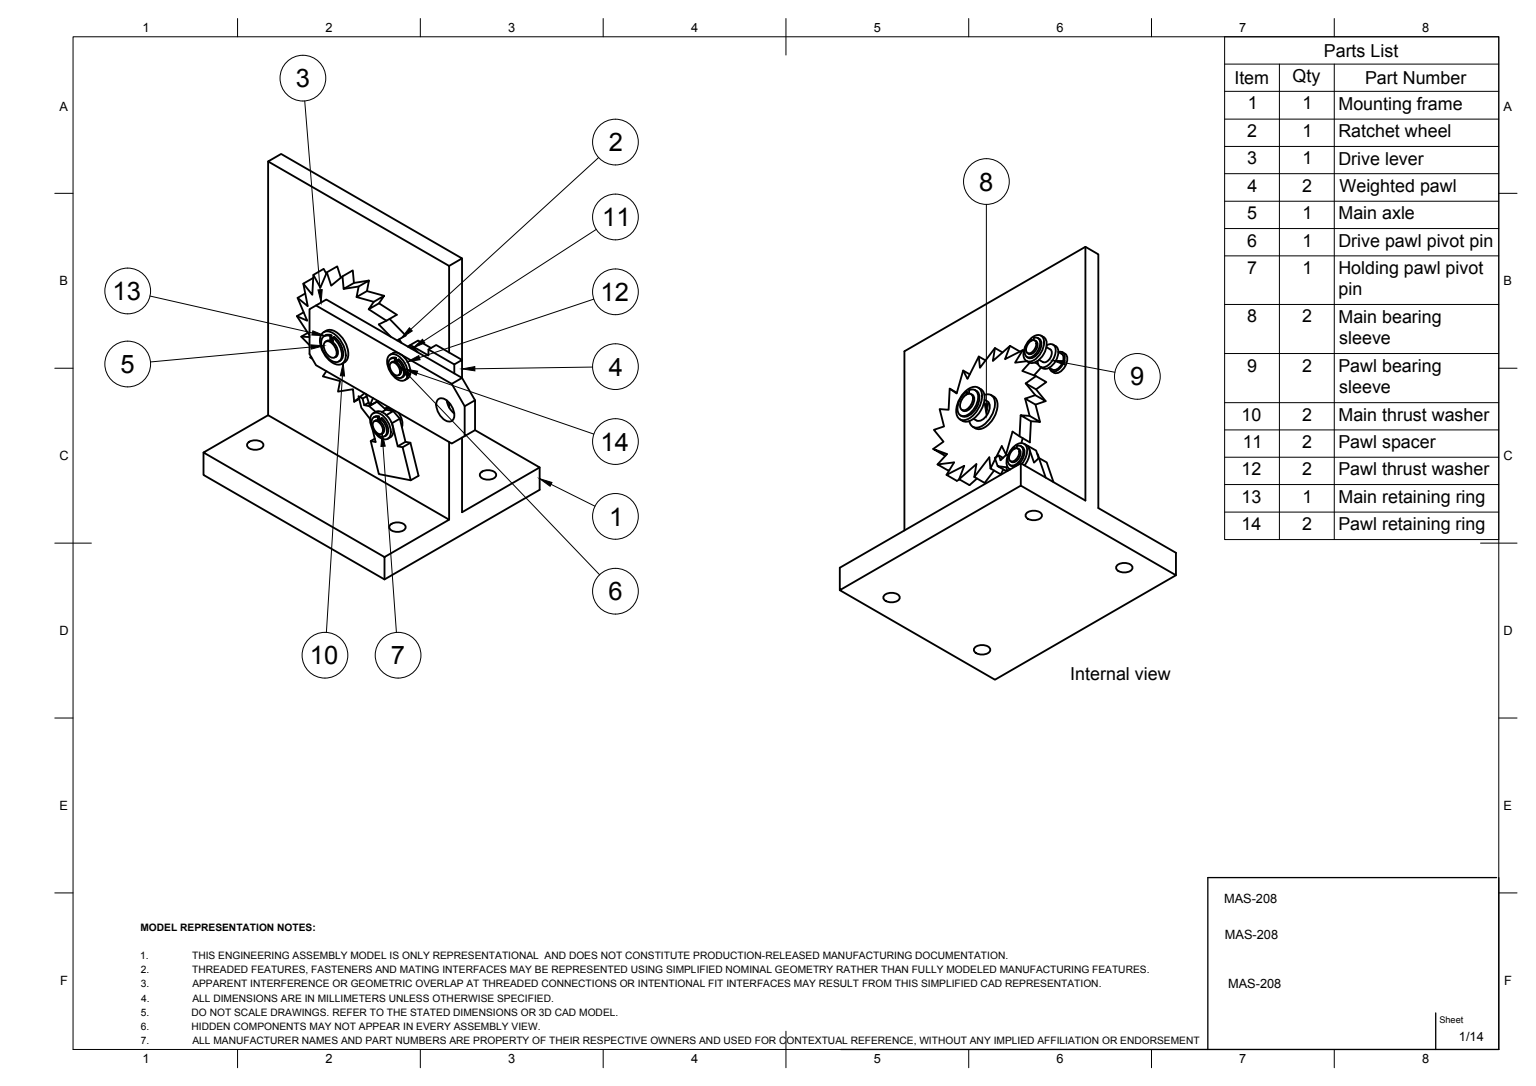
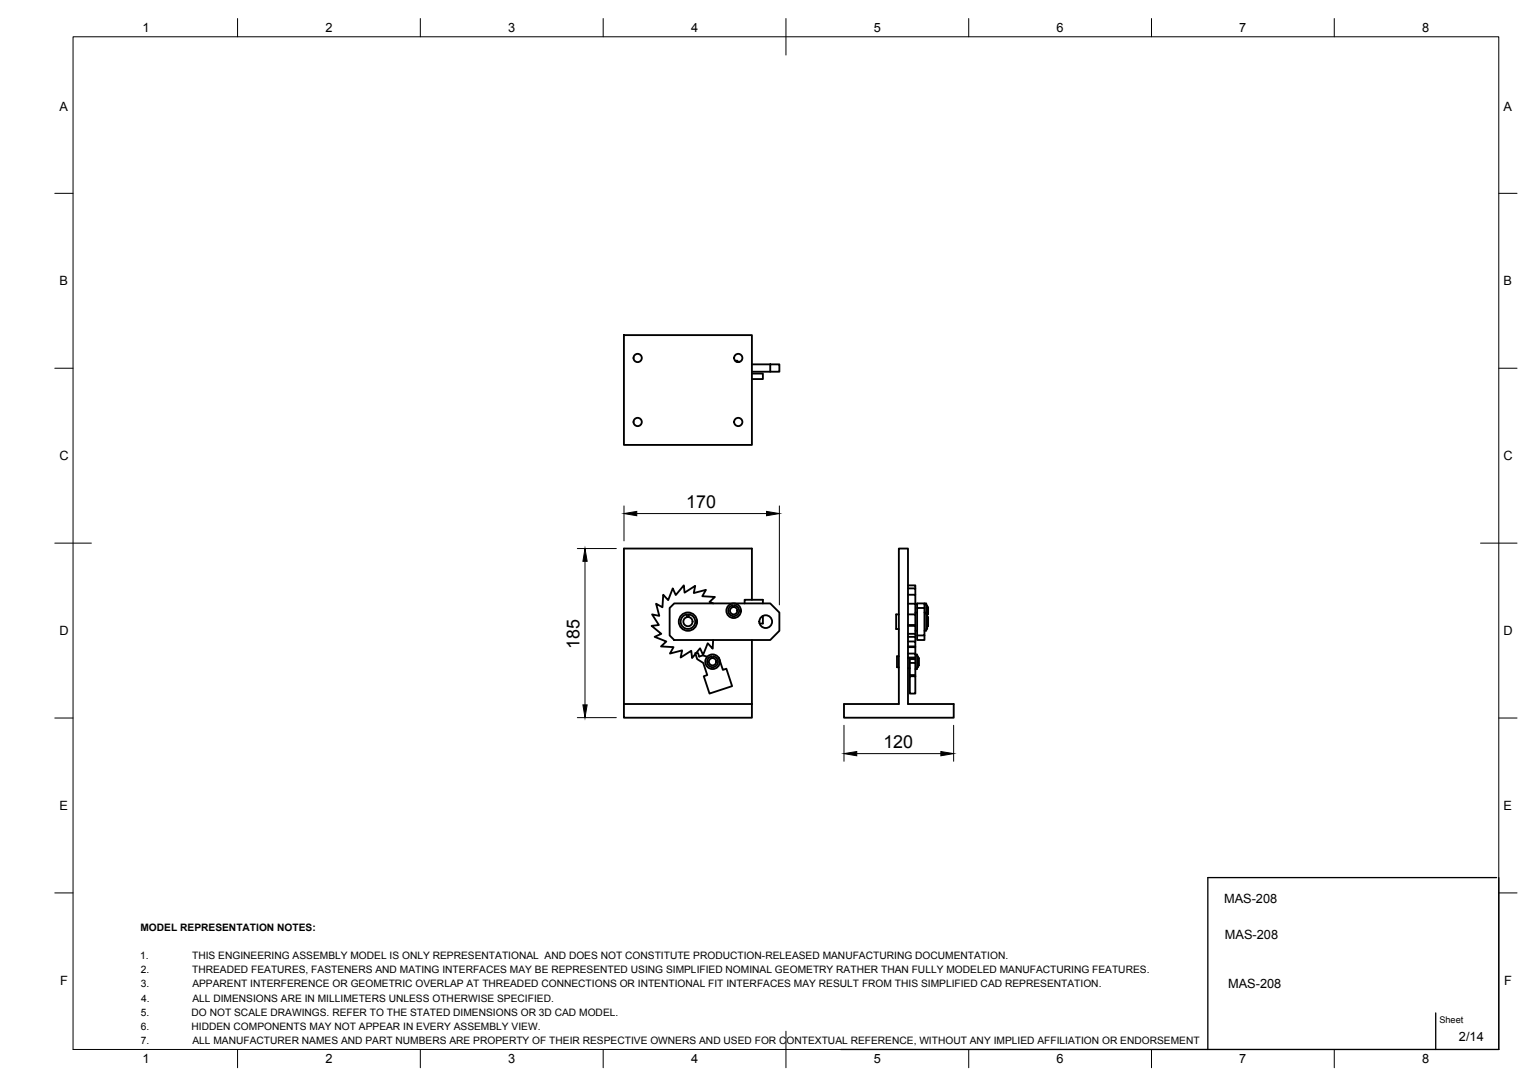
ISO-10303-21;
HEADER;
/* Generated by software containing ST-Developer
 * from STEP Tools, Inc. (www.steptools.com) 
 */

FILE_DESCRIPTION(
/* description */ ('Independent vertical20-tooth ratchet advance with repeated integral-c
ounterweight gravity pawls, swinging drive lever, bronze sleeves and f
ully retained axle stacks.18degpertooth. Native revolutes; geometric c
ycle checking rather than automatic contact/rolling dynamics. Gravity 
closing checked from actual pawl center of mass. Backplate/foot suppor
ts unit. Fits, torque, holding force, wear and life unassigned.'),
/* implementation_level */ '2;1');

FILE_NAME(
/* name */ 'MAS-208.step',
/* time_stamp */ '2026-11-09T06:25:53-08:00',
/* author */ (''),
/* organization */ (''),
/* preprocessor_version */ 'ST-DEVELOPER v20.2',
/* originating_system */ 'Autodesk Translation Framework v15.17.0.0',
/* authorisation */ '');

FILE_SCHEMA (('AUTOMOTIVE_DESIGN { 1 0 10303 214 3 1 1 }'));
ENDSEC;

DATA;
#10=MECHANICAL_DESIGN_GEOMETRIC_PRESENTATION_REPRESENTATION('',(#123,#124,
#125,#126,#127,#128,#129,#130,#131,#132,#133,#134,#135,#136),#4643);
#11=ITEM_DEFINED_TRANSFORMATION($,$,#2829,#3066);
#12=ITEM_DEFINED_TRANSFORMATION($,$,#2858,#3067);
#13=ITEM_DEFINED_TRANSFORMATION($,$,#2904,#3068);
#14=ITEM_DEFINED_TRANSFORMATION($,$,#2989,#3069);
#15=ITEM_DEFINED_TRANSFORMATION($,$,#2924,#3070);
#16=ITEM_DEFINED_TRANSFORMATION($,$,#2942,#3071);
#17=ITEM_DEFINED_TRANSFORMATION($,$,#2960,#3072);
#18=ITEM_DEFINED_TRANSFORMATION($,$,#3010,#3073);
#19=ITEM_DEFINED_TRANSFORMATION($,$,#3019,#3074);
#20=ITEM_DEFINED_TRANSFORMATION($,$,#3028,#3075);
#21=ITEM_DEFINED_TRANSFORMATION($,$,#3037,#3076);
#22=ITEM_DEFINED_TRANSFORMATION($,$,#3046,#3077);
#23=ITEM_DEFINED_TRANSFORMATION($,$,#2978,#3078);
#24=ITEM_DEFINED_TRANSFORMATION($,$,#3055,#3079);
#25=ITEM_DEFINED_TRANSFORMATION($,$,#2989,#3080);
#26=ITEM_DEFINED_TRANSFORMATION($,$,#3010,#3081);
#27=ITEM_DEFINED_TRANSFORMATION($,$,#3019,#3082);
#28=ITEM_DEFINED_TRANSFORMATION($,$,#3028,#3083);
#29=ITEM_DEFINED_TRANSFORMATION($,$,#3037,#3084);
#30=ITEM_DEFINED_TRANSFORMATION($,$,#3046,#3085);
#31=ITEM_DEFINED_TRANSFORMATION($,$,#3055,#3086);
#32=(
REPRESENTATION_RELATIONSHIP($,$,#4700,#4699)
REPRESENTATION_RELATIONSHIP_WITH_TRANSFORMATION(#11)
SHAPE_REPRESENTATION_RELATIONSHIP()
);
#33=(
REPRESENTATION_RELATIONSHIP($,$,#4701,#4699)
REPRESENTATION_RELATIONSHIP_WITH_TRANSFORMATION(#12)
SHAPE_REPRESENTATION_RELATIONSHIP()
);
#34=(
REPRESENTATION_RELATIONSHIP($,$,#4702,#4699)
REPRESENTATION_RELATIONSHIP_WITH_TRANSFORMATION(#13)
SHAPE_REPRESENTATION_RELATIONSHIP()
);
#35=(
REPRESENTATION_RELATIONSHIP($,$,#4707,#4699)
REPRESENTATION_RELATIONSHIP_WITH_TRANSFORMATION(#14)
SHAPE_REPRESENTATION_RELATIONSHIP()
);
#36=(
REPRESENTATION_RELATIONSHIP($,$,#4703,#4699)
REPRESENTATION_RELATIONSHIP_WITH_TRANSFORMATION(#15)
SHAPE_REPRESENTATION_RELATIONSHIP()
);
#37=(
REPRESENTATION_RELATIONSHIP($,$,#4704,#4699)
REPRESENTATION_RELATIONSHIP_WITH_TRANSFORMATION(#16)
SHAPE_REPRESENTATION_RELATIONSHIP()
);
#38=(
REPRESENTATION_RELATIONSHIP($,$,#4705,#4699)
REPRESENTATION_RELATIONSHIP_WITH_TRANSFORMATION(#17)
SHAPE_REPRESENTATION_RELATIONSHIP()
);
#39=(
REPRESENTATION_RELATIONSHIP($,$,#4708,#4699)
REPRESENTATION_RELATIONSHIP_WITH_TRANSFORMATION(#18)
SHAPE_REPRESENTATION_RELATIONSHIP()
);
#40=(
REPRESENTATION_RELATIONSHIP($,$,#4709,#4699)
REPRESENTATION_RELATIONSHIP_WITH_TRANSFORMATION(#19)
SHAPE_REPRESENTATION_RELATIONSHIP()
);
#41=(
REPRESENTATION_RELATIONSHIP($,$,#4710,#4699)
REPRESENTATION_RELATIONSHIP_WITH_TRANSFORMATION(#20)
SHAPE_REPRESENTATION_RELATIONSHIP()
);
#42=(
REPRESENTATION_RELATIONSHIP($,$,#4711,#4699)
REPRESENTATION_RELATIONSHIP_WITH_TRANSFORMATION(#21)
SHAPE_REPRESENTATION_RELATIONSHIP()
);
#43=(
REPRESENTATION_RELATIONSHIP($,$,#4712,#4699)
REPRESENTATION_RELATIONSHIP_WITH_TRANSFORMATION(#22)
SHAPE_REPRESENTATION_RELATIONSHIP()
);
#44=(
REPRESENTATION_RELATIONSHIP($,$,#4706,#4699)
REPRESENTATION_RELATIONSHIP_WITH_TRANSFORMATION(#23)
SHAPE_REPRESENTATION_RELATIONSHIP()
);
#45=(
REPRESENTATION_RELATIONSHIP($,$,#4713,#4699)
REPRESENTATION_RELATIONSHIP_WITH_TRANSFORMATION(#24)
SHAPE_REPRESENTATION_RELATIONSHIP()
);
#46=(
REPRESENTATION_RELATIONSHIP($,$,#4707,#4699)
REPRESENTATION_RELATIONSHIP_WITH_TRANSFORMATION(#25)
SHAPE_REPRESENTATION_RELATIONSHIP()
);
#47=(
REPRESENTATION_RELATIONSHIP($,$,#4708,#4699)
REPRESENTATION_RELATIONSHIP_WITH_TRANSFORMATION(#26)
SHAPE_REPRESENTATION_RELATIONSHIP()
);
#48=(
REPRESENTATION_RELATIONSHIP($,$,#4709,#4699)
REPRESENTATION_RELATIONSHIP_WITH_TRANSFORMATION(#27)
SHAPE_REPRESENTATION_RELATIONSHIP()
);
#49=(
REPRESENTATION_RELATIONSHIP($,$,#4710,#4699)
REPRESENTATION_RELATIONSHIP_WITH_TRANSFORMATION(#28)
SHAPE_REPRESENTATION_RELATIONSHIP()
);
#50=(
REPRESENTATION_RELATIONSHIP($,$,#4711,#4699)
REPRESENTATION_RELATIONSHIP_WITH_TRANSFORMATION(#29)
SHAPE_REPRESENTATION_RELATIONSHIP()
);
#51=(
REPRESENTATION_RELATIONSHIP($,$,#4712,#4699)
REPRESENTATION_RELATIONSHIP_WITH_TRANSFORMATION(#30)
SHAPE_REPRESENTATION_RELATIONSHIP()
);
#52=(
REPRESENTATION_RELATIONSHIP($,$,#4713,#4699)
REPRESENTATION_RELATIONSHIP_WITH_TRANSFORMATION(#31)
SHAPE_REPRESENTATION_RELATIONSHIP()
);
#53=CONTEXT_DEPENDENT_SHAPE_REPRESENTATION(#32,#4678);
#54=CONTEXT_DEPENDENT_SHAPE_REPRESENTATION(#33,#4679);
#55=CONTEXT_DEPENDENT_SHAPE_REPRESENTATION(#34,#4680);
#56=CONTEXT_DEPENDENT_SHAPE_REPRESENTATION(#35,#4681);
#57=CONTEXT_DEPENDENT_SHAPE_REPRESENTATION(#36,#4682);
#58=CONTEXT_DEPENDENT_SHAPE_REPRESENTATION(#37,#4683);
#59=CONTEXT_DEPENDENT_SHAPE_REPRESENTATION(#38,#4684);
#60=CONTEXT_DEPENDENT_SHAPE_REPRESENTATION(#39,#4685);
#61=CONTEXT_DEPENDENT_SHAPE_REPRESENTATION(#40,#4686);
#62=CONTEXT_DEPENDENT_SHAPE_REPRESENTATION(#41,#4687);
#63=CONTEXT_DEPENDENT_SHAPE_REPRESENTATION(#42,#4688);
#64=CONTEXT_DEPENDENT_SHAPE_REPRESENTATION(#43,#4689);
#65=CONTEXT_DEPENDENT_SHAPE_REPRESENTATION(#44,#4690);
#66=CONTEXT_DEPENDENT_SHAPE_REPRESENTATION(#45,#4691);
#67=CONTEXT_DEPENDENT_SHAPE_REPRESENTATION(#46,#4692);
#68=CONTEXT_DEPENDENT_SHAPE_REPRESENTATION(#47,#4693);
#69=CONTEXT_DEPENDENT_SHAPE_REPRESENTATION(#48,#4694);
#70=CONTEXT_DEPENDENT_SHAPE_REPRESENTATION(#49,#4695);
#71=CONTEXT_DEPENDENT_SHAPE_REPRESENTATION(#50,#4696);
#72=CONTEXT_DEPENDENT_SHAPE_REPRESENTATION(#51,#4697);
#73=CONTEXT_DEPENDENT_SHAPE_REPRESENTATION(#52,#4698);
#74=NEXT_ASSEMBLY_USAGE_OCCURRENCE('Mounting frame:1',
'Mounting frame:1','Mounting frame:1',#4715,#4716,'Mounting frame:1');
#75=NEXT_ASSEMBLY_USAGE_OCCURRENCE('Ratchet wheel:1','Ratchet wheel:1',
'Ratchet wheel:1',#4715,#4717,'Ratchet wheel:1');
#76=NEXT_ASSEMBLY_USAGE_OCCURRENCE('Drive lever:1','Drive lever:1',
'Drive lever:1',#4715,#4718,'Drive lever:1');
#77=NEXT_ASSEMBLY_USAGE_OCCURRENCE('Weighted pawl:1','Weighted pawl:1',
'Weighted pawl:1',#4715,#4723,'Weighted pawl:1');
#78=NEXT_ASSEMBLY_USAGE_OCCURRENCE('Main axle:1','Main axle:1',
'Main axle:1',#4715,#4719,'Main axle:1');
#79=NEXT_ASSEMBLY_USAGE_OCCURRENCE('Drive pawl pivot pin:1',
'Drive pawl pivot pin:1','Drive pawl pivot pin:1',#4715,#4720,
'Drive pawl pivot pin:1');
#80=NEXT_ASSEMBLY_USAGE_OCCURRENCE('Holding pawl pivot pin:1',
'Holding pawl pivot pin:1','Holding pawl pivot pin:1',#4715,#4721,
'Holding pawl pivot pin:1');
#81=NEXT_ASSEMBLY_USAGE_OCCURRENCE('Main bearing sleeve:1',
'Main bearing sleeve:1','Main bearing sleeve:1',#4715,#4724,
'Main bearing sleeve:1');
#82=NEXT_ASSEMBLY_USAGE_OCCURRENCE('Pawl bearing sleeve:1',
'Pawl bearing sleeve:1','Pawl bearing sleeve:1',#4715,#4725,
'Pawl bearing sleeve:1');
#83=NEXT_ASSEMBLY_USAGE_OCCURRENCE('Main thrust washer:1',
'Main thrust washer:1','Main thrust washer:1',#4715,#4726,
'Main thrust washer:1');
#84=NEXT_ASSEMBLY_USAGE_OCCURRENCE('Pawl spacer:1','Pawl spacer:1',
'Pawl spacer:1',#4715,#4727,'Pawl spacer:1');
#85=NEXT_ASSEMBLY_USAGE_OCCURRENCE('Pawl thrust washer:1',
'Pawl thrust washer:1','Pawl thrust washer:1',#4715,#4728,
'Pawl thrust washer:1');
#86=NEXT_ASSEMBLY_USAGE_OCCURRENCE('Main retaining ring:1',
'Main retaining ring:1','Main retaining ring:1',#4715,#4722,
'Main retaining ring:1');
#87=NEXT_ASSEMBLY_USAGE_OCCURRENCE('Pawl retaining ring:1',
'Pawl retaining ring:1','Pawl retaining ring:1',#4715,#4729,
'Pawl retaining ring:1');
#88=NEXT_ASSEMBLY_USAGE_OCCURRENCE('Weighted pawl:2','Weighted pawl:2',
'Weighted pawl:2',#4715,#4723,'Weighted pawl:2');
#89=NEXT_ASSEMBLY_USAGE_OCCURRENCE('Main bearing sleeve:2',
'Main bearing sleeve:2','Main bearing sleeve:2',#4715,#4724,
'Main bearing sleeve:2');
#90=NEXT_ASSEMBLY_USAGE_OCCURRENCE('Pawl bearing sleeve:2',
'Pawl bearing sleeve:2','Pawl bearing sleeve:2',#4715,#4725,
'Pawl bearing sleeve:2');
#91=NEXT_ASSEMBLY_USAGE_OCCURRENCE('Main thrust washer:2',
'Main thrust washer:2','Main thrust washer:2',#4715,#4726,
'Main thrust washer:2');
#92=NEXT_ASSEMBLY_USAGE_OCCURRENCE('Pawl spacer:2','Pawl spacer:2',
'Pawl spacer:2',#4715,#4727,'Pawl spacer:2');
#93=NEXT_ASSEMBLY_USAGE_OCCURRENCE('Pawl thrust washer:2',
'Pawl thrust washer:2','Pawl thrust washer:2',#4715,#4728,
'Pawl thrust washer:2');
#94=NEXT_ASSEMBLY_USAGE_OCCURRENCE('Pawl retaining ring:2',
'Pawl retaining ring:2','Pawl retaining ring:2',#4715,#4729,
'Pawl retaining ring:2');
#95=SHAPE_REPRESENTATION_RELATIONSHIP('SRR','None',#4700,#109);
#96=SHAPE_REPRESENTATION_RELATIONSHIP('SRR','None',#4701,#110);
#97=SHAPE_REPRESENTATION_RELATIONSHIP('SRR','None',#4702,#111);
#98=SHAPE_REPRESENTATION_RELATIONSHIP('SRR','None',#4703,#112);
#99=SHAPE_REPRESENTATION_RELATIONSHIP('SRR','None',#4704,#113);
#100=SHAPE_REPRESENTATION_RELATIONSHIP('SRR','None',#4705,#114);
#101=SHAPE_REPRESENTATION_RELATIONSHIP('SRR','None',#4706,#115);
#102=SHAPE_REPRESENTATION_RELATIONSHIP('SRR','None',#4707,#116);
#103=SHAPE_REPRESENTATION_RELATIONSHIP('SRR','None',#4708,#117);
#104=SHAPE_REPRESENTATION_RELATIONSHIP('SRR','None',#4709,#118);
#105=SHAPE_REPRESENTATION_RELATIONSHIP('SRR','None',#4710,#119);
#106=SHAPE_REPRESENTATION_RELATIONSHIP('SRR','None',#4711,#120);
#107=SHAPE_REPRESENTATION_RELATIONSHIP('SRR','None',#4712,#121);
#108=SHAPE_REPRESENTATION_RELATIONSHIP('SRR','None',#4713,#122);
#109=ADVANCED_BREP_SHAPE_REPRESENTATION('',(#137),#4629);
#110=ADVANCED_BREP_SHAPE_REPRESENTATION('',(#138),#4630);
#111=ADVANCED_BREP_SHAPE_REPRESENTATION('',(#139),#4631);
#112=ADVANCED_BREP_SHAPE_REPRESENTATION('',(#140),#4632);
#113=ADVANCED_BREP_SHAPE_REPRESENTATION('',(#141),#4633);
#114=ADVANCED_BREP_SHAPE_REPRESENTATION('',(#142),#4634);
#115=ADVANCED_BREP_SHAPE_REPRESENTATION('',(#143),#4635);
#116=ADVANCED_BREP_SHAPE_REPRESENTATION('',(#144),#4636);
#117=ADVANCED_BREP_SHAPE_REPRESENTATION('',(#145),#4637);
#118=ADVANCED_BREP_SHAPE_REPRESENTATION('',(#146),#4638);
#119=ADVANCED_BREP_SHAPE_REPRESENTATION('',(#147),#4639);
#120=ADVANCED_BREP_SHAPE_REPRESENTATION('',(#148),#4640);
#121=ADVANCED_BREP_SHAPE_REPRESENTATION('',(#149),#4641);
#122=ADVANCED_BREP_SHAPE_REPRESENTATION('',(#150),#4642);
#123=STYLED_ITEM('',(#4779),#137);
#124=STYLED_ITEM('',(#4780),#138);
#125=STYLED_ITEM('',(#4781),#139);
#126=STYLED_ITEM('',(#4782),#140);
#127=STYLED_ITEM('',(#4782),#141);
#128=STYLED_ITEM('',(#4782),#142);
#129=STYLED_ITEM('',(#4783),#143);
#130=STYLED_ITEM('',(#4784),#144);
#131=STYLED_ITEM('',(#4785),#145);
#132=STYLED_ITEM('',(#4785),#146);
#133=STYLED_ITEM('',(#4786),#147);
#134=STYLED_ITEM('',(#4786),#148);
#135=STYLED_ITEM('',(#4786),#149);
#136=STYLED_ITEM('',(#4783),#150);
#137=MANIFOLD_SOLID_BREP('Body1',#2659);
#138=MANIFOLD_SOLID_BREP('Body1',#2660);
#139=MANIFOLD_SOLID_BREP('Body1',#2661);
#140=MANIFOLD_SOLID_BREP('Body1',#2662);
#141=MANIFOLD_SOLID_BREP('Body1',#2663);
#142=MANIFOLD_SOLID_BREP('Body1',#2664);
#143=MANIFOLD_SOLID_BREP('Body1',#2665);
#144=MANIFOLD_SOLID_BREP('Body1',#2666);
#145=MANIFOLD_SOLID_BREP('Body1',#2667);
#146=MANIFOLD_SOLID_BREP('Body1',#2668);
#147=MANIFOLD_SOLID_BREP('Body1',#2669);
#148=MANIFOLD_SOLID_BREP('Body1',#2670);
#149=MANIFOLD_SOLID_BREP('Body1',#2671);
#150=MANIFOLD_SOLID_BREP('Body1',#2672);
#151=FACE_BOUND('',#460,.T.);
#152=FACE_BOUND('',#461,.T.);
#153=FACE_BOUND('',#463,.T.);
#154=FACE_BOUND('',#464,.T.);
#155=FACE_BOUND('',#466,.T.);
#156=FACE_BOUND('',#467,.T.);
#157=FACE_BOUND('',#468,.T.);
#158=FACE_BOUND('',#469,.T.);
#159=FACE_BOUND('',#476,.T.);
#160=FACE_BOUND('',#477,.T.);
#161=FACE_BOUND('',#479,.T.);
#162=FACE_BOUND('',#480,.T.);
#163=FACE_BOUND('',#523,.T.);
#164=FACE_BOUND('',#525,.T.);
#165=FACE_BOUND('',#538,.T.);
#166=FACE_BOUND('',#539,.T.);
#167=FACE_BOUND('',#540,.T.);
#168=FACE_BOUND('',#542,.T.);
#169=FACE_BOUND('',#543,.T.);
#170=FACE_BOUND('',#544,.T.);
#171=FACE_BOUND('',#547,.T.);
#172=FACE_BOUND('',#549,.T.);
#173=FACE_BOUND('',#552,.T.);
#174=FACE_BOUND('',#559,.T.);
#175=FACE_BOUND('',#561,.T.);
#176=FACE_BOUND('',#564,.T.);
#177=FACE_BOUND('',#571,.T.);
#178=FACE_BOUND('',#573,.T.);
#179=FACE_BOUND('',#576,.T.);
#180=FACE_BOUND('',#604,.T.);
#181=FACE_BOUND('',#606,.T.);
#182=FACE_BOUND('',#610,.T.);
#183=FACE_BOUND('',#612,.T.);
#184=FACE_BOUND('',#616,.T.);
#185=FACE_BOUND('',#618,.T.);
#186=FACE_BOUND('',#622,.T.);
#187=FACE_BOUND('',#624,.T.);
#188=FACE_BOUND('',#628,.T.);
#189=FACE_BOUND('',#630,.T.);
#190=FACE_BOUND('',#634,.T.);
#191=FACE_BOUND('',#636,.T.);
#192=PLANE('',#2848);
#193=PLANE('',#2849);
#194=PLANE('',#2850);
#195=PLANE('',#2851);
#196=PLANE('',#2852);
#197=PLANE('',#2853);
#198=PLANE('',#2854);
#199=PLANE('',#2855);
#200=PLANE('',#2856);
#201=PLANE('',#2857);
#202=PLANE('',#2862);
#203=PLANE('',#2863);
#204=PLANE('',#2864);
#205=PLANE('',#2865);
#206=PLANE('',#2866);
#207=PLANE('',#2867);
#208=PLANE('',#2868);
#209=PLANE('',#2869);
#210=PLANE('',#2870);
#211=PLANE('',#2871);
#212=PLANE('',#2872);
#213=PLANE('',#2873);
#214=PLANE('',#2874);
#215=PLANE('',#2875);
#216=PLANE('',#2876);
#217=PLANE('',#2877);
#218=PLANE('',#2878);
#219=PLANE('',#2879);
#220=PLANE('',#2880);
#221=PLANE('',#2881);
#222=PLANE('',#2882);
#223=PLANE('',#2883);
#224=PLANE('',#2884);
#225=PLANE('',#2885);
#226=PLANE('',#2886);
#227=PLANE('',#2887);
#228=PLANE('',#2888);
#229=PLANE('',#2889);
#230=PLANE('',#2890);
#231=PLANE('',#2891);
#232=PLANE('',#2892);
#233=PLANE('',#2893);
#234=PLANE('',#2894);
#235=PLANE('',#2895);
#236=PLANE('',#2896);
#237=PLANE('',#2897);
#238=PLANE('',#2898);
#239=PLANE('',#2899);
#240=PLANE('',#2900);
#241=PLANE('',#2901);
#242=PLANE('',#2902);
#243=PLANE('',#2903);
#244=PLANE('',#2914);
#245=PLANE('',#2915);
#246=PLANE('',#2916);
#247=PLANE('',#2917);
#248=PLANE('',#2918);
#249=PLANE('',#2919);
#250=PLANE('',#2920);
#251=PLANE('',#2921);
#252=PLANE('',#2922);
#253=PLANE('',#2923);
#254=PLANE('',#2928);
#255=PLANE('',#2930);
#256=PLANE('',#2934);
#257=PLANE('',#2939);
#258=PLANE('',#2941);
#259=PLANE('',#2946);
#260=PLANE('',#2948);
#261=PLANE('',#2952);
#262=PLANE('',#2957);
#263=PLANE('',#2959);
#264=PLANE('',#2964);
#265=PLANE('',#2966);
#266=PLANE('',#2970);
#267=PLANE('',#2975);
#268=PLANE('',#2977);
#269=PLANE('',#2979);
#270=PLANE('',#2980);
#271=PLANE('',#2981);
#272=PLANE('',#2988);
#273=PLANE('',#2993);
#274=PLANE('',#2994);
#275=PLANE('',#2995);
#276=PLANE('',#2996);
#277=PLANE('',#2997);
#278=PLANE('',#2998);
#279=PLANE('',#2999);
#280=PLANE('',#3000);
#281=PLANE('',#3001);
#282=PLANE('',#3002);
#283=PLANE('',#3003);
#284=PLANE('',#3004);
#285=PLANE('',#3005);
#286=PLANE('',#3006);
#287=PLANE('',#3007);
#288=PLANE('',#3008);
#289=PLANE('',#3009);
#290=PLANE('',#3017);
#291=PLANE('',#3018);
#292=PLANE('',#3026);
#293=PLANE('',#3027);
#294=PLANE('',#3035);
#295=PLANE('',#3036);
#296=PLANE('',#3044);
#297=PLANE('',#3045);
#298=PLANE('',#3053);
#299=PLANE('',#3054);
#300=PLANE('',#3056);
#301=PLANE('',#3057);
#302=PLANE('',#3058);
#303=PLANE('',#3065);
#304=FACE_OUTER_BOUND('',#453,.T.);
#305=FACE_OUTER_BOUND('',#454,.T.);
#306=FACE_OUTER_BOUND('',#455,.T.);
#307=FACE_OUTER_BOUND('',#456,.T.);
#308=FACE_OUTER_BOUND('',#457,.T.);
#309=FACE_OUTER_BOUND('',#458,.T.);
#310=FACE_OUTER_BOUND('',#459,.T.);
#311=FACE_OUTER_BOUND('',#462,.T.);
#312=FACE_OUTER_BOUND('',#465,.T.);
#313=FACE_OUTER_BOUND('',#470,.T.);
#314=FACE_OUTER_BOUND('',#471,.T.);
#315=FACE_OUTER_BOUND('',#472,.T.);
#316=FACE_OUTER_BOUND('',#473,.T.);
#317=FACE_OUTER_BOUND('',#474,.T.);
#318=FACE_OUTER_BOUND('',#475,.T.);
#319=FACE_OUTER_BOUND('',#478,.T.);
#320=FACE_OUTER_BOUND('',#481,.T.);
#321=FACE_OUTER_BOUND('',#482,.T.);
#322=FACE_OUTER_BOUND('',#483,.T.);
#323=FACE_OUTER_BOUND('',#484,.T.);
#324=FACE_OUTER_BOUND('',#485,.T.);
#325=FACE_OUTER_BOUND('',#486,.T.);
#326=FACE_OUTER_BOUND('',#487,.T.);
#327=FACE_OUTER_BOUND('',#488,.T.);
#328=FACE_OUTER_BOUND('',#489,.T.);
#329=FACE_OUTER_BOUND('',#490,.T.);
#330=FACE_OUTER_BOUND('',#491,.T.);
#331=FACE_OUTER_BOUND('',#492,.T.);
#332=FACE_OUTER_BOUND('',#493,.T.);
#333=FACE_OUTER_BOUND('',#494,.T.);
#334=FACE_OUTER_BOUND('',#495,.T.);
#335=FACE_OUTER_BOUND('',#496,.T.);
#336=FACE_OUTER_BOUND('',#497,.T.);
#337=FACE_OUTER_BOUND('',#498,.T.);
#338=FACE_OUTER_BOUND('',#499,.T.);
#339=FACE_OUTER_BOUND('',#500,.T.);
#340=FACE_OUTER_BOUND('',#501,.T.);
#341=FACE_OUTER_BOUND('',#502,.T.);
#342=FACE_OUTER_BOUND('',#503,.T.);
#343=FACE_OUTER_BOUND('',#504,.T.);
#344=FACE_OUTER_BOUND('',#505,.T.);
#345=FACE_OUTER_BOUND('',#506,.T.);
#346=FACE_OUTER_BOUND('',#507,.T.);
#347=FACE_OUTER_BOUND('',#508,.T.);
#348=FACE_OUTER_BOUND('',#509,.T.);
#349=FACE_OUTER_BOUND('',#510,.T.);
#350=FACE_OUTER_BOUND('',#511,.T.);
#351=FACE_OUTER_BOUND('',#512,.T.);
#352=FACE_OUTER_BOUND('',#513,.T.);
#353=FACE_OUTER_BOUND('',#514,.T.);
#354=FACE_OUTER_BOUND('',#515,.T.);
#355=FACE_OUTER_BOUND('',#516,.T.);
#356=FACE_OUTER_BOUND('',#517,.T.);
#357=FACE_OUTER_BOUND('',#518,.T.);
#358=FACE_OUTER_BOUND('',#519,.T.);
#359=FACE_OUTER_BOUND('',#520,.T.);
#360=FACE_OUTER_BOUND('',#521,.T.);
#361=FACE_OUTER_BOUND('',#522,.T.);
#362=FACE_OUTER_BOUND('',#524,.T.);
#363=FACE_OUTER_BOUND('',#526,.T.);
#364=FACE_OUTER_BOUND('',#527,.T.);
#365=FACE_OUTER_BOUND('',#528,.T.);
#366=FACE_OUTER_BOUND('',#529,.T.);
#367=FACE_OUTER_BOUND('',#530,.T.);
#368=FACE_OUTER_BOUND('',#531,.T.);
#369=FACE_OUTER_BOUND('',#532,.T.);
#370=FACE_OUTER_BOUND('',#533,.T.);
#371=FACE_OUTER_BOUND('',#534,.T.);
#372=FACE_OUTER_BOUND('',#535,.T.);
#373=FACE_OUTER_BOUND('',#536,.T.);
#374=FACE_OUTER_BOUND('',#537,.T.);
#375=FACE_OUTER_BOUND('',#541,.T.);
#376=FACE_OUTER_BOUND('',#545,.T.);
#377=FACE_OUTER_BOUND('',#546,.T.);
#378=FACE_OUTER_BOUND('',#548,.T.);
#379=FACE_OUTER_BOUND('',#550,.T.);
#380=FACE_OUTER_BOUND('',#551,.T.);
#381=FACE_OUTER_BOUND('',#553,.T.);
#382=FACE_OUTER_BOUND('',#554,.T.);
#383=FACE_OUTER_BOUND('',#555,.T.);
#384=FACE_OUTER_BOUND('',#556,.T.);
#385=FACE_OUTER_BOUND('',#557,.T.);
#386=FACE_OUTER_BOUND('',#558,.T.);
#387=FACE_OUTER_BOUND('',#560,.T.);
#388=FACE_OUTER_BOUND('',#562,.T.);
#389=FACE_OUTER_BOUND('',#563,.T.);
#390=FACE_OUTER_BOUND('',#565,.T.);
#391=FACE_OUTER_BOUND('',#566,.T.);
#392=FACE_OUTER_BOUND('',#567,.T.);
#393=FACE_OUTER_BOUND('',#568,.T.);
#394=FACE_OUTER_BOUND('',#569,.T.);
#395=FACE_OUTER_BOUND('',#570,.T.);
#396=FACE_OUTER_BOUND('',#572,.T.);
#397=FACE_OUTER_BOUND('',#574,.T.);
#398=FACE_OUTER_BOUND('',#575,.T.);
#399=FACE_OUTER_BOUND('',#577,.T.);
#400=FACE_OUTER_BOUND('',#578,.T.);
#401=FACE_OUTER_BOUND('',#579,.T.);
#402=FACE_OUTER_BOUND('',#580,.T.);
#403=FACE_OUTER_BOUND('',#581,.T.);
#404=FACE_OUTER_BOUND('',#582,.T.);
#405=FACE_OUTER_BOUND('',#583,.T.);
#406=FACE_OUTER_BOUND('',#584,.T.);
#407=FACE_OUTER_BOUND('',#585,.T.);
#408=FACE_OUTER_BOUND('',#586,.T.);
#409=FACE_OUTER_BOUND('',#587,.T.);
#410=FACE_OUTER_BOUND('',#588,.T.);
#411=FACE_OUTER_BOUND('',#589,.T.);
#412=FACE_OUTER_BOUND('',#590,.T.);
#413=FACE_OUTER_BOUND('',#591,.T.);
#414=FACE_OUTER_BOUND('',#592,.T.);
#415=FACE_OUTER_BOUND('',#593,.T.);
#416=FACE_OUTER_BOUND('',#594,.T.);
#417=FACE_OUTER_BOUND('',#595,.T.);
#418=FACE_OUTER_BOUND('',#596,.T.);
#419=FACE_OUTER_BOUND('',#597,.T.);
#420=FACE_OUTER_BOUND('',#598,.T.);
#421=FACE_OUTER_BOUND('',#599,.T.);
#422=FACE_OUTER_BOUND('',#600,.T.);
#423=FACE_OUTER_BOUND('',#601,.T.);
#424=FACE_OUTER_BOUND('',#602,.T.);
#425=FACE_OUTER_BOUND('',#603,.T.);
#426=FACE_OUTER_BOUND('',#605,.T.);
#427=FACE_OUTER_BOUND('',#607,.T.);
#428=FACE_OUTER_BOUND('',#608,.T.);
#429=FACE_OUTER_BOUND('',#609,.T.);
#430=FACE_OUTER_BOUND('',#611,.T.);
#431=FACE_OUTER_BOUND('',#613,.T.);
#432=FACE_OUTER_BOUND('',#614,.T.);
#433=FACE_OUTER_BOUND('',#615,.T.);
#434=FACE_OUTER_BOUND('',#617,.T.);
#435=FACE_OUTER_BOUND('',#619,.T.);
#436=FACE_OUTER_BOUND('',#620,.T.);
#437=FACE_OUTER_BOUND('',#621,.T.);
#438=FACE_OUTER_BOUND('',#623,.T.);
#439=FACE_OUTER_BOUND('',#625,.T.);
#440=FACE_OUTER_BOUND('',#626,.T.);
#441=FACE_OUTER_BOUND('',#627,.T.);
#442=FACE_OUTER_BOUND('',#629,.T.);
#443=FACE_OUTER_BOUND('',#631,.T.);
#444=FACE_OUTER_BOUND('',#632,.T.);
#445=FACE_OUTER_BOUND('',#633,.T.);
#446=FACE_OUTER_BOUND('',#635,.T.);
#447=FACE_OUTER_BOUND('',#637,.T.);
#448=FACE_OUTER_BOUND('',#638,.T.);
#449=FACE_OUTER_BOUND('',#639,.T.);
#450=FACE_OUTER_BOUND('',#640,.T.);
#451=FACE_OUTER_BOUND('',#641,.T.);
#452=FACE_OUTER_BOUND('',#642,.T.);
#453=EDGE_LOOP('',(#1801,#1802,#1803,#1804));
#454=EDGE_LOOP('',(#1805,#1806,#1807,#1808));
#455=EDGE_LOOP('',(#1809,#1810,#1811,#1812));
#456=EDGE_LOOP('',(#1813,#1814,#1815,#1816));
#457=EDGE_LOOP('',(#1817,#1818,#1819,#1820));
#458=EDGE_LOOP('',(#1821,#1822,#1823,#1824));
#459=EDGE_LOOP('',(#1825,#1826,#1827,#1828));
#460=EDGE_LOOP('',(#1829));
#461=EDGE_LOOP('',(#1830));
#462=EDGE_LOOP('',(#1831,#1832,#1833,#1834));
#463=EDGE_LOOP('',(#1835));
#464=EDGE_LOOP('',(#1836));
#465=EDGE_LOOP('',(#1837,#1838,#1839,#1840));
#466=EDGE_LOOP('',(#1841));
#467=EDGE_LOOP('',(#1842));
#468=EDGE_LOOP('',(#1843));
#469=EDGE_LOOP('',(#1844));
#470=EDGE_LOOP('',(#1845,#1846,#1847,#1848));
#471=EDGE_LOOP('',(#1849,#1850,#1851,#1852));
#472=EDGE_LOOP('',(#1853,#1854,#1855,#1856));
#473=EDGE_LOOP('',(#1857,#1858,#1859,#1860,#1861,#1862,#1863,#1864));
#474=EDGE_LOOP('',(#1865,#1866,#1867,#1868,#1869,#1870,#1871,#1872));
#475=EDGE_LOOP('',(#1873,#1874,#1875,#1876));
#476=EDGE_LOOP('',(#1877));
#477=EDGE_LOOP('',(#1878));
#478=EDGE_LOOP('',(#1879,#1880,#1881,#1882));
#479=EDGE_LOOP('',(#1883));
#480=EDGE_LOOP('',(#1884));
#481=EDGE_LOOP('',(#1885,#1886,#1887,#1888));
#482=EDGE_LOOP('',(#1889,#1890,#1891,#1892));
#483=EDGE_LOOP('',(#1893,#1894,#1895,#1896));
#484=EDGE_LOOP('',(#1897,#1898,#1899,#1900));
#485=EDGE_LOOP('',(#1901,#1902,#1903,#1904));
#486=EDGE_LOOP('',(#1905,#1906,#1907,#1908));
#487=EDGE_LOOP('',(#1909,#1910,#1911,#1912));
#488=EDGE_LOOP('',(#1913,#1914,#1915,#1916));
#489=EDGE_LOOP('',(#1917,#1918,#1919,#1920));
#490=EDGE_LOOP('',(#1921,#1922,#1923,#1924));
#491=EDGE_LOOP('',(#1925,#1926,#1927,#1928));
#492=EDGE_LOOP('',(#1929,#1930,#1931,#1932));
#493=EDGE_LOOP('',(#1933,#1934,#1935,#1936));
#494=EDGE_LOOP('',(#1937,#1938,#1939,#1940));
#495=EDGE_LOOP('',(#1941,#1942,#1943,#1944));
#496=EDGE_LOOP('',(#1945,#1946,#1947,#1948));
#497=EDGE_LOOP('',(#1949,#1950,#1951,#1952));
#498=EDGE_LOOP('',(#1953,#1954,#1955,#1956));
#499=EDGE_LOOP('',(#1957,#1958,#1959,#1960));
#500=EDGE_LOOP('',(#1961,#1962,#1963,#1964));
#501=EDGE_LOOP('',(#1965,#1966,#1967,#1968));
#502=EDGE_LOOP('',(#1969,#1970,#1971,#1972));
#503=EDGE_LOOP('',(#1973,#1974,#1975,#1976));
#504=EDGE_LOOP('',(#1977,#1978,#1979,#1980));
#505=EDGE_LOOP('',(#1981,#1982,#1983,#1984));
#506=EDGE_LOOP('',(#1985,#1986,#1987,#1988));
#507=EDGE_LOOP('',(#1989,#1990,#1991,#1992));
#508=EDGE_LOOP('',(#1993,#1994,#1995,#1996));
#509=EDGE_LOOP('',(#1997,#1998,#1999,#2000));
#510=EDGE_LOOP('',(#2001,#2002,#2003,#2004));
#511=EDGE_LOOP('',(#2005,#2006,#2007,#2008));
#512=EDGE_LOOP('',(#2009,#2010,#2011,#2012));
#513=EDGE_LOOP('',(#2013,#2014,#2015,#2016));
#514=EDGE_LOOP('',(#2017,#2018,#2019,#2020));
#515=EDGE_LOOP('',(#2021,#2022,#2023,#2024));
#516=EDGE_LOOP('',(#2025,#2026,#2027,#2028));
#517=EDGE_LOOP('',(#2029,#2030,#2031,#2032));
#518=EDGE_LOOP('',(#2033,#2034,#2035,#2036));
#519=EDGE_LOOP('',(#2037,#2038,#2039,#2040));
#520=EDGE_LOOP('',(#2041,#2042,#2043,#2044));
#521=EDGE_LOOP('',(#2045,#2046,#2047,#2048));
#522=EDGE_LOOP('',(#2049,#2050,#2051,#2052,#2053,#2054,#2055,#2056,#2057,
#2058,#2059,#2060,#2061,#2062,#2063,#2064,#2065,#2066,#2067,#2068,#2069,
#2070,#2071,#2072,#2073,#2074,#2075,#2076,#2077,#2078,#2079,#2080,#2081,
#2082,#2083,#2084,#2085,#2086,#2087,#2088));
#523=EDGE_LOOP('',(#2089));
#524=EDGE_LOOP('',(#2090,#2091,#2092,#2093,#2094,#2095,#2096,#2097,#2098,
#2099,#2100,#2101,#2102,#2103,#2104,#2105,#2106,#2107,#2108,#2109,#2110,
#2111,#2112,#2113,#2114,#2115,#2116,#2117,#2118,#2119,#2120,#2121,#2122,
#2123,#2124,#2125,#2126,#2127,#2128,#2129));
#525=EDGE_LOOP('',(#2130));
#526=EDGE_LOOP('',(#2131,#2132,#2133,#2134));
#527=EDGE_LOOP('',(#2135,#2136,#2137,#2138));
#528=EDGE_LOOP('',(#2139,#2140,#2141,#2142));
#529=EDGE_LOOP('',(#2143,#2144,#2145,#2146));
#530=EDGE_LOOP('',(#2147,#2148,#2149,#2150));
#531=EDGE_LOOP('',(#2151,#2152,#2153,#2154));
#532=EDGE_LOOP('',(#2155,#2156,#2157,#2158));
#533=EDGE_LOOP('',(#2159,#2160,#2161,#2162));
#534=EDGE_LOOP('',(#2163,#2164,#2165,#2166));
#535=EDGE_LOOP('',(#2167,#2168,#2169,#2170));
#536=EDGE_LOOP('',(#2171,#2172,#2173,#2174));
#537=EDGE_LOOP('',(#2175,#2176,#2177,#2178,#2179,#2180,#2181,#2182));
#538=EDGE_LOOP('',(#2183));
#539=EDGE_LOOP('',(#2184));
#540=EDGE_LOOP('',(#2185));
#541=EDGE_LOOP('',(#2186,#2187,#2188,#2189,#2190,#2191,#2192,#2193));
#542=EDGE_LOOP('',(#2194));
#543=EDGE_LOOP('',(#2195));
#544=EDGE_LOOP('',(#2196));
#545=EDGE_LOOP('',(#2197,#2198,#2199,#2200));
#546=EDGE_LOOP('',(#2201));
#547=EDGE_LOOP('',(#2202));
#548=EDGE_LOOP('',(#2203));
#549=EDGE_LOOP('',(#2204));
#550=EDGE_LOOP('',(#2205,#2206,#2207,#2208));
#551=EDGE_LOOP('',(#2209));
#552=EDGE_LOOP('',(#2210));
#553=EDGE_LOOP('',(#2211,#2212,#2213,#2214));
#554=EDGE_LOOP('',(#2215));
#555=EDGE_LOOP('',(#2216,#2217,#2218,#2219));
#556=EDGE_LOOP('',(#2220));
#557=EDGE_LOOP('',(#2221,#2222,#2223,#2224));
#558=EDGE_LOOP('',(#2225));
#559=EDGE_LOOP('',(#2226));
#560=EDGE_LOOP('',(#2227));
#561=EDGE_LOOP('',(#2228));
#562=EDGE_LOOP('',(#2229,#2230,#2231,#2232));
#563=EDGE_LOOP('',(#2233));
#564=EDGE_LOOP('',(#2234));
#565=EDGE_LOOP('',(#2235,#2236,#2237,#2238));
#566=EDGE_LOOP('',(#2239));
#567=EDGE_LOOP('',(#2240,#2241,#2242,#2243));
#568=EDGE_LOOP('',(#2244));
#569=EDGE_LOOP('',(#2245,#2246,#2247,#2248));
#570=EDGE_LOOP('',(#2249));
#571=EDGE_LOOP('',(#2250));
#572=EDGE_LOOP('',(#2251));
#573=EDGE_LOOP('',(#2252));
#574=EDGE_LOOP('',(#2253,#2254,#2255,#2256));
#575=EDGE_LOOP('',(#2257));
#576=EDGE_LOOP('',(#2258));
#577=EDGE_LOOP('',(#2259,#2260,#2261,#2262));
#578=EDGE_LOOP('',(#2263));
#579=EDGE_LOOP('',(#2264,#2265,#2266,#2267));
#580=EDGE_LOOP('',(#2268));
#581=EDGE_LOOP('',(#2269,#2270,#2271,#2272));
#582=EDGE_LOOP('',(#2273,#2274,#2275,#2276));
#583=EDGE_LOOP('',(#2277,#2278,#2279,#2280));
#584=EDGE_LOOP('',(#2281,#2282,#2283,#2284));
#585=EDGE_LOOP('',(#2285,#2286,#2287,#2288));
#586=EDGE_LOOP('',(#2289,#2290,#2291,#2292));
#587=EDGE_LOOP('',(#2293,#2294,#2295,#2296));
#588=EDGE_LOOP('',(#2297,#2298,#2299,#2300));
#589=EDGE_LOOP('',(#2301,#2302,#2303,#2304));
#590=EDGE_LOOP('',(#2305,#2306,#2307,#2308));
#591=EDGE_LOOP('',(#2309,#2310,#2311,#2312));
#592=EDGE_LOOP('',(#2313,#2314,#2315,#2316));
#593=EDGE_LOOP('',(#2317,#2318,#2319,#2320));
#594=EDGE_LOOP('',(#2321,#2322,#2323,#2324));
#595=EDGE_LOOP('',(#2325,#2326,#2327,#2328));
#596=EDGE_LOOP('',(#2329,#2330,#2331,#2332));
#597=EDGE_LOOP('',(#2333,#2334,#2335,#2336));
#598=EDGE_LOOP('',(#2337,#2338,#2339,#2340));
#599=EDGE_LOOP('',(#2341,#2342,#2343,#2344));
#600=EDGE_LOOP('',(#2345,#2346,#2347,#2348));
#601=EDGE_LOOP('',(#2349,#2350,#2351,#2352));
#602=EDGE_LOOP('',(#2353,#2354,#2355,#2356));
#603=EDGE_LOOP('',(#2357,#2358,#2359,#2360,#2361,#2362,#2363,#2364,#2365,
#2366,#2367,#2368,#2369,#2370,#2371));
#604=EDGE_LOOP('',(#2372));
#605=EDGE_LOOP('',(#2373,#2374,#2375,#2376,#2377,#2378,#2379,#2380,#2381,
#2382,#2383,#2384,#2385,#2386,#2387));
#606=EDGE_LOOP('',(#2388));
#607=EDGE_LOOP('',(#2389,#2390,#2391,#2392));
#608=EDGE_LOOP('',(#2393,#2394,#2395,#2396));
#609=EDGE_LOOP('',(#2397));
#610=EDGE_LOOP('',(#2398));
#611=EDGE_LOOP('',(#2399));
#612=EDGE_LOOP('',(#2400));
#613=EDGE_LOOP('',(#2401,#2402,#2403,#2404));
#614=EDGE_LOOP('',(#2405,#2406,#2407,#2408));
#615=EDGE_LOOP('',(#2409));
#616=EDGE_LOOP('',(#2410));
#617=EDGE_LOOP('',(#2411));
#618=EDGE_LOOP('',(#2412));
#619=EDGE_LOOP('',(#2413,#2414,#2415,#2416));
#620=EDGE_LOOP('',(#2417,#2418,#2419,#2420));
#621=EDGE_LOOP('',(#2421));
#622=EDGE_LOOP('',(#2422));
#623=EDGE_LOOP('',(#2423));
#624=EDGE_LOOP('',(#2424));
#625=EDGE_LOOP('',(#2425,#2426,#2427,#2428));
#626=EDGE_LOOP('',(#2429,#2430,#2431,#2432));
#627=EDGE_LOOP('',(#2433));
#628=EDGE_LOOP('',(#2434));
#629=EDGE_LOOP('',(#2435));
#630=EDGE_LOOP('',(#2436));
#631=EDGE_LOOP('',(#2437,#2438,#2439,#2440));
#632=EDGE_LOOP('',(#2441,#2442,#2443,#2444));
#633=EDGE_LOOP('',(#2445));
#634=EDGE_LOOP('',(#2446));
#635=EDGE_LOOP('',(#2447));
#636=EDGE_LOOP('',(#2448));
#637=EDGE_LOOP('',(#2449,#2450,#2451,#2452));
#638=EDGE_LOOP('',(#2453,#2454,#2455,#2456));
#639=EDGE_LOOP('',(#2457,#2458,#2459,#2460));
#640=EDGE_LOOP('',(#2461,#2462,#2463,#2464));
#641=EDGE_LOOP('',(#2465,#2466,#2467,#2468));
#642=EDGE_LOOP('',(#2469,#2470,#2471,#2472));
#643=LINE('',#3873,#905);
#644=LINE('',#3879,#906);
#645=LINE('',#3885,#907);
#646=LINE('',#3891,#908);
#647=LINE('',#3897,#909);
#648=LINE('',#3903,#910);
#649=LINE('',#3908,#911);
#650=LINE('',#3910,#912);
#651=LINE('',#3912,#913);
#652=LINE('',#3913,#914);
#653=LINE('',#3917,#915);
#654=LINE('',#3919,#916);
#655=LINE('',#3921,#917);
#656=LINE('',#3922,#918);
#657=LINE('',#3926,#919);
#658=LINE('',#3928,#920);
#659=LINE('',#3930,#921);
#660=LINE('',#3931,#922);
#661=LINE('',#3933,#923);
#662=LINE('',#3934,#924);
#663=LINE('',#3936,#925);
#664=LINE('',#3937,#926);
#665=LINE('',#3941,#927);
#666=LINE('',#3943,#928);
#667=LINE('',#3945,#929);
#668=LINE('',#3946,#930);
#669=LINE('',#3948,#931);
#670=LINE('',#3949,#932);
#671=LINE('',#3951,#933);
#672=LINE('',#3952,#934);
#673=LINE('',#3960,#935);
#674=LINE('',#3965,#936);
#675=LINE('',#3967,#937);
#676=LINE('',#3969,#938);
#677=LINE('',#3970,#939);
#678=LINE('',#3973,#940);
#679=LINE('',#3975,#941);
#680=LINE('',#3976,#942);
#681=LINE('',#3979,#943);
#682=LINE('',#3981,#944);
#683=LINE('',#3982,#945);
#684=LINE('',#3985,#946);
#685=LINE('',#3987,#947);
#686=LINE('',#3988,#948);
#687=LINE('',#3991,#949);
#688=LINE('',#3993,#950);
#689=LINE('',#3994,#951);
#690=LINE('',#3997,#952);
#691=LINE('',#3999,#953);
#692=LINE('',#4000,#954);
#693=LINE('',#4003,#955);
#694=LINE('',#4005,#956);
#695=LINE('',#4006,#957);
#696=LINE('',#4009,#958);
#697=LINE('',#4011,#959);
#698=LINE('',#4012,#960);
#699=LINE('',#4015,#961);
#700=LINE('',#4017,#962);
#701=LINE('',#4018,#963);
#702=LINE('',#4021,#964);
#703=LINE('',#4023,#965);
#704=LINE('',#4024,#966);
#705=LINE('',#4027,#967);
#706=LINE('',#4029,#968);
#707=LINE('',#4030,#969);
#708=LINE('',#4033,#970);
#709=LINE('',#4035,#971);
#710=LINE('',#4036,#972);
#711=LINE('',#4039,#973);
#712=LINE('',#4041,#974);
#713=LINE('',#4042,#975);
#714=LINE('',#4045,#976);
#715=LINE('',#4047,#977);
#716=LINE('',#4048,#978);
#717=LINE('',#4051,#979);
#718=LINE('',#4053,#980);
#719=LINE('',#4054,#981);
#720=LINE('',#4057,#982);
#721=LINE('',#4059,#983);
#722=LINE('',#4060,#984);
#723=LINE('',#4063,#985);
#724=LINE('',#4065,#986);
#725=LINE('',#4066,#987);
#726=LINE('',#4069,#988);
#727=LINE('',#4071,#989);
#728=LINE('',#4072,#990);
#729=LINE('',#4075,#991);
#730=LINE('',#4077,#992);
#731=LINE('',#4078,#993);
#732=LINE('',#4081,#994);
#733=LINE('',#4083,#995);
#734=LINE('',#4084,#996);
#735=LINE('',#4087,#997);
#736=LINE('',#4089,#998);
#737=LINE('',#4090,#999);
#738=LINE('',#4093,#1000);
#739=LINE('',#4095,#1001);
#740=LINE('',#4096,#1002);
#741=LINE('',#4099,#1003);
#742=LINE('',#4101,#1004);
#743=LINE('',#4102,#1005);
#744=LINE('',#4105,#1006);
#745=LINE('',#4107,#1007);
#746=LINE('',#4108,#1008);
#747=LINE('',#4111,#1009);
#748=LINE('',#4113,#1010);
#749=LINE('',#4114,#1011);
#750=LINE('',#4117,#1012);
#751=LINE('',#4119,#1013);
#752=LINE('',#4120,#1014);
#753=LINE('',#4123,#1015);
#754=LINE('',#4125,#1016);
#755=LINE('',#4126,#1017);
#756=LINE('',#4129,#1018);
#757=LINE('',#4131,#1019);
#758=LINE('',#4132,#1020);
#759=LINE('',#4135,#1021);
#760=LINE('',#4137,#1022);
#761=LINE('',#4138,#1023);
#762=LINE('',#4141,#1024);
#763=LINE('',#4143,#1025);
#764=LINE('',#4144,#1026);
#765=LINE('',#4147,#1027);
#766=LINE('',#4149,#1028);
#767=LINE('',#4150,#1029);
#768=LINE('',#4153,#1030);
#769=LINE('',#4155,#1031);
#770=LINE('',#4156,#1032);
#771=LINE('',#4159,#1033);
#772=LINE('',#4161,#1034);
#773=LINE('',#4162,#1035);
#774=LINE('',#4165,#1036);
#775=LINE('',#4167,#1037);
#776=LINE('',#4168,#1038);
#777=LINE('',#4171,#1039);
#778=LINE('',#4173,#1040);
#779=LINE('',#4174,#1041);
#780=LINE('',#4177,#1042);
#781=LINE('',#4179,#1043);
#782=LINE('',#4180,#1044);
#783=LINE('',#4183,#1045);
#784=LINE('',#4185,#1046);
#785=LINE('',#4186,#1047);
#786=LINE('',#4189,#1048);
#787=LINE('',#4191,#1049);
#788=LINE('',#4192,#1050);
#789=LINE('',#4195,#1051);
#790=LINE('',#4197,#1052);
#791=LINE('',#4198,#1053);
#792=LINE('',#4200,#1054);
#793=LINE('',#4201,#1055);
#794=LINE('',#4209,#1056);
#795=LINE('',#4215,#1057);
#796=LINE('',#4221,#1058);
#797=LINE('',#4226,#1059);
#798=LINE('',#4228,#1060);
#799=LINE('',#4230,#1061);
#800=LINE('',#4231,#1062);
#801=LINE('',#4234,#1063);
#802=LINE('',#4236,#1064);
#803=LINE('',#4237,#1065);
#804=LINE('',#4240,#1066);
#805=LINE('',#4242,#1067);
#806=LINE('',#4243,#1068);
#807=LINE('',#4246,#1069);
#808=LINE('',#4248,#1070);
#809=LINE('',#4249,#1071);
#810=LINE('',#4252,#1072);
#811=LINE('',#4254,#1073);
#812=LINE('',#4255,#1074);
#813=LINE('',#4258,#1075);
#814=LINE('',#4260,#1076);
#815=LINE('',#4261,#1077);
#816=LINE('',#4264,#1078);
#817=LINE('',#4266,#1079);
#818=LINE('',#4267,#1080);
#819=LINE('',#4269,#1081);
#820=LINE('',#4270,#1082);
#821=LINE('',#4278,#1083);
#822=LINE('',#4289,#1084);
#823=LINE('',#4297,#1085);
#824=LINE('',#4301,#1086);
#825=LINE('',#4308,#1087);
#826=LINE('',#4319,#1088);
#827=LINE('',#4327,#1089);
#828=LINE('',#4331,#1090);
#829=LINE('',#4338,#1091);
#830=LINE('',#4349,#1092);
#831=LINE('',#4357,#1093);
#832=LINE('',#4361,#1094);
#833=LINE('',#4367,#1095);
#834=LINE('',#4369,#1096);
#835=LINE('',#4371,#1097);
#836=LINE('',#4372,#1098);
#837=LINE('',#4376,#1099);
#838=LINE('',#4378,#1100);
#839=LINE('',#4380,#1101);
#840=LINE('',#4381,#1102);
#841=LINE('',#4395,#1103);
#842=LINE('',#4400,#1104);
#843=LINE('',#4402,#1105);
#844=LINE('',#4404,#1106);
#845=LINE('',#4405,#1107);
#846=LINE('',#4408,#1108);
#847=LINE('',#4410,#1109);
#848=LINE('',#4411,#1110);
#849=LINE('',#4414,#1111);
#850=LINE('',#4416,#1112);
#851=LINE('',#4417,#1113);
#852=LINE('',#4420,#1114);
#853=LINE('',#4422,#1115);
#854=LINE('',#4423,#1116);
#855=LINE('',#4426,#1117);
#856=LINE('',#4428,#1118);
#857=LINE('',#4429,#1119);
#858=LINE('',#4432,#1120);
#859=LINE('',#4434,#1121);
#860=LINE('',#4435,#1122);
#861=LINE('',#4438,#1123);
#862=LINE('',#4440,#1124);
#863=LINE('',#4441,#1125);
#864=LINE('',#4444,#1126);
#865=LINE('',#4446,#1127);
#866=LINE('',#4447,#1128);
#867=LINE('',#4450,#1129);
#868=LINE('',#4452,#1130);
#869=LINE('',#4453,#1131);
#870=LINE('',#4456,#1132);
#871=LINE('',#4458,#1133);
#872=LINE('',#4459,#1134);
#873=LINE('',#4462,#1135);
#874=LINE('',#4464,#1136);
#875=LINE('',#4465,#1137);
#876=LINE('',#4468,#1138);
#877=LINE('',#4470,#1139);
#878=LINE('',#4471,#1140);
#879=LINE('',#4474,#1141);
#880=LINE('',#4476,#1142);
#881=LINE('',#4477,#1143);
#882=LINE('',#4480,#1144);
#883=LINE('',#4482,#1145);
#884=LINE('',#4483,#1146);
#885=LINE('',#4485,#1147);
#886=LINE('',#4486,#1148);
#887=LINE('',#4494,#1149);
#888=LINE('',#4500,#1150);
#889=LINE('',#4509,#1151);
#890=LINE('',#4515,#1152);
#891=LINE('',#4524,#1153);
#892=LINE('',#4530,#1154);
#893=LINE('',#4539,#1155);
#894=LINE('',#4545,#1156);
#895=LINE('',#4554,#1157);
#896=LINE('',#4560,#1158);
#897=LINE('',#4568,#1159);
#898=LINE('',#4570,#1160);
#899=LINE('',#4572,#1161);
#900=LINE('',#4573,#1162);
#901=LINE('',#4577,#1163);
#902=LINE('',#4579,#1164);
#903=LINE('',#4581,#1165);
#904=LINE('',#4582,#1166);
#905=VECTOR('',#3095,4.);
#906=VECTOR('',#3102,5.);
#907=VECTOR('',#3109,4.5);
#908=VECTOR('',#3116,4.5);
#909=VECTOR('',#3123,4.5);
#910=VECTOR('',#3130,4.5);
#911=VECTOR('',#3135,10.);
#912=VECTOR('',#3136,10.);
#913=VECTOR('',#3137,10.);
#914=VECTOR('',#3138,10.);
#915=VECTOR('',#3141,10.);
#916=VECTOR('',#3142,10.);
#917=VECTOR('',#3143,10.);
#918=VECTOR('',#3144,10.);
#919=VECTOR('',#3147,10.);
#920=VECTOR('',#3148,10.);
#921=VECTOR('',#3149,10.);
#922=VECTOR('',#3150,10.);
#923=VECTOR('',#3153,10.);
#924=VECTOR('',#3154,10.);
#925=VECTOR('',#3157,10.);
#926=VECTOR('',#3158,10.);
#927=VECTOR('',#3161,10.);
#928=VECTOR('',#3162,10.);
#929=VECTOR('',#3163,10.);
#930=VECTOR('',#3164,10.);
#931=VECTOR('',#3167,10.);
#932=VECTOR('',#3168,10.);
#933=VECTOR('',#3171,10.);
#934=VECTOR('',#3172,10.);
#935=VECTOR('',#3183,6.);
#936=VECTOR('',#3188,10.);
#937=VECTOR('',#3189,10.);
#938=VECTOR('',#3190,10.);
#939=VECTOR('',#3191,10.);
#940=VECTOR('',#3194,10.);
#941=VECTOR('',#3195,10.);
#942=VECTOR('',#3196,10.);
#943=VECTOR('',#3199,10.);
#944=VECTOR('',#3200,10.);
#945=VECTOR('',#3201,10.);
#946=VECTOR('',#3204,10.);
#947=VECTOR('',#3205,10.);
#948=VECTOR('',#3206,10.);
#949=VECTOR('',#3209,10.);
#950=VECTOR('',#3210,10.);
#951=VECTOR('',#3211,10.);
#952=VECTOR('',#3214,10.);
#953=VECTOR('',#3215,10.);
#954=VECTOR('',#3216,10.);
#955=VECTOR('',#3219,10.);
#956=VECTOR('',#3220,10.);
#957=VECTOR('',#3221,10.);
#958=VECTOR('',#3224,10.);
#959=VECTOR('',#3225,10.);
#960=VECTOR('',#3226,10.);
#961=VECTOR('',#3229,10.);
#962=VECTOR('',#3230,10.);
#963=VECTOR('',#3231,10.);
#964=VECTOR('',#3234,10.);
#965=VECTOR('',#3235,10.);
#966=VECTOR('',#3236,10.);
#967=VECTOR('',#3239,10.);
#968=VECTOR('',#3240,10.);
#969=VECTOR('',#3241,10.);
#970=VECTOR('',#3244,10.);
#971=VECTOR('',#3245,10.);
#972=VECTOR('',#3246,10.);
#973=VECTOR('',#3249,10.);
#974=VECTOR('',#3250,10.);
#975=VECTOR('',#3251,10.);
#976=VECTOR('',#3254,10.);
#977=VECTOR('',#3255,10.);
#978=VECTOR('',#3256,10.);
#979=VECTOR('',#3259,10.);
#980=VECTOR('',#3260,10.);
#981=VECTOR('',#3261,10.);
#982=VECTOR('',#3264,10.);
#983=VECTOR('',#3265,10.);
#984=VECTOR('',#3266,10.);
#985=VECTOR('',#3269,10.);
#986=VECTOR('',#3270,10.);
#987=VECTOR('',#3271,10.);
#988=VECTOR('',#3274,10.);
#989=VECTOR('',#3275,10.);
#990=VECTOR('',#3276,10.);
#991=VECTOR('',#3279,10.);
#992=VECTOR('',#3280,10.);
#993=VECTOR('',#3281,10.);
#994=VECTOR('',#3284,10.);
#995=VECTOR('',#3285,10.);
#996=VECTOR('',#3286,10.);
#997=VECTOR('',#3289,10.);
#998=VECTOR('',#3290,10.);
#999=VECTOR('',#3291,10.);
#1000=VECTOR('',#3294,10.);
#1001=VECTOR('',#3295,10.);
#1002=VECTOR('',#3296,10.);
#1003=VECTOR('',#3299,10.);
#1004=VECTOR('',#3300,10.);
#1005=VECTOR('',#3301,10.);
#1006=VECTOR('',#3304,10.);
#1007=VECTOR('',#3305,10.);
#1008=VECTOR('',#3306,10.);
#1009=VECTOR('',#3309,10.);
#1010=VECTOR('',#3310,10.);
#1011=VECTOR('',#3311,10.);
#1012=VECTOR('',#3314,10.);
#1013=VECTOR('',#3315,10.);
#1014=VECTOR('',#3316,10.);
#1015=VECTOR('',#3319,10.);
#1016=VECTOR('',#3320,10.);
#1017=VECTOR('',#3321,10.);
#1018=VECTOR('',#3324,10.);
#1019=VECTOR('',#3325,10.);
#1020=VECTOR('',#3326,10.);
#1021=VECTOR('',#3329,10.);
#1022=VECTOR('',#3330,10.);
#1023=VECTOR('',#3331,10.);
#1024=VECTOR('',#3334,10.);
#1025=VECTOR('',#3335,10.);
#1026=VECTOR('',#3336,10.);
#1027=VECTOR('',#3339,10.);
#1028=VECTOR('',#3340,10.);
#1029=VECTOR('',#3341,10.);
#1030=VECTOR('',#3344,10.);
#1031=VECTOR('',#3345,10.);
#1032=VECTOR('',#3346,10.);
#1033=VECTOR('',#3349,10.);
#1034=VECTOR('',#3350,10.);
#1035=VECTOR('',#3351,10.);
#1036=VECTOR('',#3354,10.);
#1037=VECTOR('',#3355,10.);
#1038=VECTOR('',#3356,10.);
#1039=VECTOR('',#3359,10.);
#1040=VECTOR('',#3360,10.);
#1041=VECTOR('',#3361,10.);
#1042=VECTOR('',#3364,10.);
#1043=VECTOR('',#3365,10.);
#1044=VECTOR('',#3366,10.);
#1045=VECTOR('',#3369,10.);
#1046=VECTOR('',#3370,10.);
#1047=VECTOR('',#3371,10.);
#1048=VECTOR('',#3374,10.);
#1049=VECTOR('',#3375,10.);
#1050=VECTOR('',#3376,10.);
#1051=VECTOR('',#3379,10.);
#1052=VECTOR('',#3380,10.);
#1053=VECTOR('',#3381,10.);
#1054=VECTOR('',#3384,10.);
#1055=VECTOR('',#3385,10.);
#1056=VECTOR('',#3396,7.);
#1057=VECTOR('',#3403,4.);
#1058=VECTOR('',#3410,6.);
#1059=VECTOR('',#3415,10.);
#1060=VECTOR('',#3416,10.);
#1061=VECTOR('',#3417,10.);
#1062=VECTOR('',#3418,10.);
#1063=VECTOR('',#3421,10.);
#1064=VECTOR('',#3422,10.);
#1065=VECTOR('',#3423,10.);
#1066=VECTOR('',#3426,10.);
#1067=VECTOR('',#3427,10.);
#1068=VECTOR('',#3428,10.);
#1069=VECTOR('',#3431,10.);
#1070=VECTOR('',#3432,10.);
#1071=VECTOR('',#3433,10.);
#1072=VECTOR('',#3436,10.);
#1073=VECTOR('',#3437,10.);
#1074=VECTOR('',#3438,10.);
#1075=VECTOR('',#3441,10.);
#1076=VECTOR('',#3442,10.);
#1077=VECTOR('',#3443,10.);
#1078=VECTOR('',#3446,10.);
#1079=VECTOR('',#3447,10.);
#1080=VECTOR('',#3448,10.);
#1081=VECTOR('',#3451,10.);
#1082=VECTOR('',#3452,10.);
#1083=VECTOR('',#3463,4.);
#1084=VECTOR('',#3478,5.);
#1085=VECTOR('',#3487,8.);
#1086=VECTOR('',#3494,5.);
#1087=VECTOR('',#3503,3.);
#1088=VECTOR('',#3518,4.);
#1089=VECTOR('',#3527,6.);
#1090=VECTOR('',#3534,4.);
#1091=VECTOR('',#3543,3.);
#1092=VECTOR('',#3558,4.);
#1093=VECTOR('',#3567,6.);
#1094=VECTOR('',#3574,4.);
#1095=VECTOR('',#3581,10.);
#1096=VECTOR('',#3582,10.);
#1097=VECTOR('',#3583,10.);
#1098=VECTOR('',#3584,10.);
#1099=VECTOR('',#3587,10.);
#1100=VECTOR('',#3588,10.);
#1101=VECTOR('',#3589,10.);
#1102=VECTOR('',#3590,10.);
#1103=VECTOR('',#3613,5.);
#1104=VECTOR('',#3618,10.);
#1105=VECTOR('',#3619,10.);
#1106=VECTOR('',#3620,10.);
#1107=VECTOR('',#3621,10.);
#1108=VECTOR('',#3624,10.);
#1109=VECTOR('',#3625,10.);
#1110=VECTOR('',#3626,10.);
#1111=VECTOR('',#3629,10.);
#1112=VECTOR('',#3630,10.);
#1113=VECTOR('',#3631,10.);
#1114=VECTOR('',#3634,10.);
#1115=VECTOR('',#3635,10.);
#1116=VECTOR('',#3636,10.);
#1117=VECTOR('',#3639,10.);
#1118=VECTOR('',#3640,10.);
#1119=VECTOR('',#3641,10.);
#1120=VECTOR('',#3644,10.);
#1121=VECTOR('',#3645,10.);
#1122=VECTOR('',#3646,10.);
#1123=VECTOR('',#3649,10.);
#1124=VECTOR('',#3650,10.);
#1125=VECTOR('',#3651,10.);
#1126=VECTOR('',#3654,10.);
#1127=VECTOR('',#3655,10.);
#1128=VECTOR('',#3656,10.);
#1129=VECTOR('',#3659,10.);
#1130=VECTOR('',#3660,10.);
#1131=VECTOR('',#3661,10.);
#1132=VECTOR('',#3664,10.);
#1133=VECTOR('',#3665,10.);
#1134=VECTOR('',#3666,10.);
#1135=VECTOR('',#3669,10.);
#1136=VECTOR('',#3670,10.);
#1137=VECTOR('',#3671,10.);
#1138=VECTOR('',#3674,10.);
#1139=VECTOR('',#3675,10.);
#1140=VECTOR('',#3676,10.);
#1141=VECTOR('',#3679,10.);
#1142=VECTOR('',#3680,10.);
#1143=VECTOR('',#3681,10.);
#1144=VECTOR('',#3684,10.);
#1145=VECTOR('',#3685,10.);
#1146=VECTOR('',#3686,10.);
#1147=VECTOR('',#3689,10.);
#1148=VECTOR('',#3690,10.);
#1149=VECTOR('',#3701,5.);
#1150=VECTOR('',#3708,6.);
#1151=VECTOR('',#3721,4.);
#1152=VECTOR('',#3728,5.);
#1153=VECTOR('',#3741,5.);
#1154=VECTOR('',#3748,10.);
#1155=VECTOR('',#3761,4.);
#1156=VECTOR('',#3768,7.);
#1157=VECTOR('',#3781,4.);
#1158=VECTOR('',#3788,8.);
#1159=VECTOR('',#3799,10.);
#1160=VECTOR('',#3800,10.);
#1161=VECTOR('',#3801,10.);
#1162=VECTOR('',#3802,10.);
#1163=VECTOR('',#3805,10.);
#1164=VECTOR('',#3806,10.);
#1165=VECTOR('',#3807,10.);
#1166=VECTOR('',#3808,10.);
#1167=CIRCLE('',#2831,4.);
#1168=CIRCLE('',#2832,4.);
#1169=CIRCLE('',#2834,5.);
#1170=CIRCLE('',#2835,5.);
#1171=CIRCLE('',#2837,4.5);
#1172=CIRCLE('',#2838,4.5);
#1173=CIRCLE('',#2840,4.5);
#1174=CIRCLE('',#2841,4.5);
#1175=CIRCLE('',#2843,4.5);
#1176=CIRCLE('',#2844,4.5);
#1177=CIRCLE('',#2846,4.5);
#1178=CIRCLE('',#2847,4.5);
#1179=CIRCLE('',#2860,6.);
#1180=CIRCLE('',#2861,6.);
#1181=CIRCLE('',#2906,7.);
#1182=CIRCLE('',#2907,7.);
#1183=CIRCLE('',#2909,4.);
#1184=CIRCLE('',#2910,4.);
#1185=CIRCLE('',#2912,6.);
#1186=CIRCLE('',#2913,6.);
#1187=CIRCLE('',#2926,4.);
#1188=CIRCLE('',#2927,4.);
#1189=CIRCLE('',#2929,5.);
#1190=CIRCLE('',#2931,5.);
#1191=CIRCLE('',#2933,5.);
#1192=CIRCLE('',#2935,8.);
#1193=CIRCLE('',#2936,5.);
#1194=CIRCLE('',#2938,8.);
#1195=CIRCLE('',#2944,3.);
#1196=CIRCLE('',#2945,3.);
#1197=CIRCLE('',#2947,4.);
#1198=CIRCLE('',#2949,4.);
#1199=CIRCLE('',#2951,4.);
#1200=CIRCLE('',#2953,6.);
#1201=CIRCLE('',#2954,4.);
#1202=CIRCLE('',#2956,6.);
#1203=CIRCLE('',#2962,3.);
#1204=CIRCLE('',#2963,3.);
#1205=CIRCLE('',#2965,4.);
#1206=CIRCLE('',#2967,4.);
#1207=CIRCLE('',#2969,4.);
#1208=CIRCLE('',#2971,6.);
#1209=CIRCLE('',#2972,4.);
#1210=CIRCLE('',#2974,6.);
#1211=CIRCLE('',#2982,8.);
#1212=CIRCLE('',#2983,4.);
#1213=CIRCLE('',#2985,4.);
#1214=CIRCLE('',#2987,8.);
#1215=CIRCLE('',#2991,5.);
#1216=CIRCLE('',#2992,5.);
#1217=CIRCLE('',#3012,5.);
#1218=CIRCLE('',#3013,5.);
#1219=CIRCLE('',#3015,6.);
#1220=CIRCLE('',#3016,6.);
#1221=CIRCLE('',#3021,4.);
#1222=CIRCLE('',#3022,4.);
#1223=CIRCLE('',#3024,5.);
#1224=CIRCLE('',#3025,5.);
#1225=CIRCLE('',#3030,5.);
#1226=CIRCLE('',#3031,5.);
#1227=CIRCLE('',#3033,10.);
#1228=CIRCLE('',#3034,10.);
#1229=CIRCLE('',#3039,4.);
#1230=CIRCLE('',#3040,4.);
#1231=CIRCLE('',#3042,7.);
#1232=CIRCLE('',#3043,7.);
#1233=CIRCLE('',#3048,4.);
#1234=CIRCLE('',#3049,4.);
#1235=CIRCLE('',#3051,8.);
#1236=CIRCLE('',#3052,8.);
#1237=CIRCLE('',#3059,6.);
#1238=CIRCLE('',#3060,3.);
#1239=CIRCLE('',#3062,3.);
#1240=CIRCLE('',#3064,6.);
#1241=VERTEX_POINT('',#3870);
#1242=VERTEX_POINT('',#3872);
#1243=VERTEX_POINT('',#3876);
#1244=VERTEX_POINT('',#3878);
#1245=VERTEX_POINT('',#3882);
#1246=VERTEX_POINT('',#3884);
#1247=VERTEX_POINT('',#3888);
#1248=VERTEX_POINT('',#3890);
#1249=VERTEX_POINT('',#3894);
#1250=VERTEX_POINT('',#3896);
#1251=VERTEX_POINT('',#3900);
#1252=VERTEX_POINT('',#3902);
#1253=VERTEX_POINT('',#3906);
#1254=VERTEX_POINT('',#3907);
#1255=VERTEX_POINT('',#3909);
#1256=VERTEX_POINT('',#3911);
#1257=VERTEX_POINT('',#3915);
#1258=VERTEX_POINT('',#3916);
#1259=VERTEX_POINT('',#3918);
#1260=VERTEX_POINT('',#3920);
#1261=VERTEX_POINT('',#3924);
#1262=VERTEX_POINT('',#3925);
#1263=VERTEX_POINT('',#3927);
#1264=VERTEX_POINT('',#3929);
#1265=VERTEX_POINT('',#3939);
#1266=VERTEX_POINT('',#3940);
#1267=VERTEX_POINT('',#3942);
#1268=VERTEX_POINT('',#3944);
#1269=VERTEX_POINT('',#3957);
#1270=VERTEX_POINT('',#3959);
#1271=VERTEX_POINT('',#3963);
#1272=VERTEX_POINT('',#3964);
#1273=VERTEX_POINT('',#3966);
#1274=VERTEX_POINT('',#3968);
#1275=VERTEX_POINT('',#3972);
#1276=VERTEX_POINT('',#3974);
#1277=VERTEX_POINT('',#3978);
#1278=VERTEX_POINT('',#3980);
#1279=VERTEX_POINT('',#3984);
#1280=VERTEX_POINT('',#3986);
#1281=VERTEX_POINT('',#3990);
#1282=VERTEX_POINT('',#3992);
#1283=VERTEX_POINT('',#3996);
#1284=VERTEX_POINT('',#3998);
#1285=VERTEX_POINT('',#4002);
#1286=VERTEX_POINT('',#4004);
#1287=VERTEX_POINT('',#4008);
#1288=VERTEX_POINT('',#4010);
#1289=VERTEX_POINT('',#4014);
#1290=VERTEX_POINT('',#4016);
#1291=VERTEX_POINT('',#4020);
#1292=VERTEX_POINT('',#4022);
#1293=VERTEX_POINT('',#4026);
#1294=VERTEX_POINT('',#4028);
#1295=VERTEX_POINT('',#4032);
#1296=VERTEX_POINT('',#4034);
#1297=VERTEX_POINT('',#4038);
#1298=VERTEX_POINT('',#4040);
#1299=VERTEX_POINT('',#4044);
#1300=VERTEX_POINT('',#4046);
#1301=VERTEX_POINT('',#4050);
#1302=VERTEX_POINT('',#4052);
#1303=VERTEX_POINT('',#4056);
#1304=VERTEX_POINT('',#4058);
#1305=VERTEX_POINT('',#4062);
#1306=VERTEX_POINT('',#4064);
#1307=VERTEX_POINT('',#4068);
#1308=VERTEX_POINT('',#4070);
#1309=VERTEX_POINT('',#4074);
#1310=VERTEX_POINT('',#4076);
#1311=VERTEX_POINT('',#4080);
#1312=VERTEX_POINT('',#4082);
#1313=VERTEX_POINT('',#4086);
#1314=VERTEX_POINT('',#4088);
#1315=VERTEX_POINT('',#4092);
#1316=VERTEX_POINT('',#4094);
#1317=VERTEX_POINT('',#4098);
#1318=VERTEX_POINT('',#4100);
#1319=VERTEX_POINT('',#4104);
#1320=VERTEX_POINT('',#4106);
#1321=VERTEX_POINT('',#4110);
#1322=VERTEX_POINT('',#4112);
#1323=VERTEX_POINT('',#4116);
#1324=VERTEX_POINT('',#4118);
#1325=VERTEX_POINT('',#4122);
#1326=VERTEX_POINT('',#4124);
#1327=VERTEX_POINT('',#4128);
#1328=VERTEX_POINT('',#4130);
#1329=VERTEX_POINT('',#4134);
#1330=VERTEX_POINT('',#4136);
#1331=VERTEX_POINT('',#4140);
#1332=VERTEX_POINT('',#4142);
#1333=VERTEX_POINT('',#4146);
#1334=VERTEX_POINT('',#4148);
#1335=VERTEX_POINT('',#4152);
#1336=VERTEX_POINT('',#4154);
#1337=VERTEX_POINT('',#4158);
#1338=VERTEX_POINT('',#4160);
#1339=VERTEX_POINT('',#4164);
#1340=VERTEX_POINT('',#4166);
#1341=VERTEX_POINT('',#4170);
#1342=VERTEX_POINT('',#4172);
#1343=VERTEX_POINT('',#4176);
#1344=VERTEX_POINT('',#4178);
#1345=VERTEX_POINT('',#4182);
#1346=VERTEX_POINT('',#4184);
#1347=VERTEX_POINT('',#4188);
#1348=VERTEX_POINT('',#4190);
#1349=VERTEX_POINT('',#4194);
#1350=VERTEX_POINT('',#4196);
#1351=VERTEX_POINT('',#4206);
#1352=VERTEX_POINT('',#4208);
#1353=VERTEX_POINT('',#4212);
#1354=VERTEX_POINT('',#4214);
#1355=VERTEX_POINT('',#4218);
#1356=VERTEX_POINT('',#4220);
#1357=VERTEX_POINT('',#4224);
#1358=VERTEX_POINT('',#4225);
#1359=VERTEX_POINT('',#4227);
#1360=VERTEX_POINT('',#4229);
#1361=VERTEX_POINT('',#4233);
#1362=VERTEX_POINT('',#4235);
#1363=VERTEX_POINT('',#4239);
#1364=VERTEX_POINT('',#4241);
#1365=VERTEX_POINT('',#4245);
#1366=VERTEX_POINT('',#4247);
#1367=VERTEX_POINT('',#4251);
#1368=VERTEX_POINT('',#4253);
#1369=VERTEX_POINT('',#4257);
#1370=VERTEX_POINT('',#4259);
#1371=VERTEX_POINT('',#4263);
#1372=VERTEX_POINT('',#4265);
#1373=VERTEX_POINT('',#4275);
#1374=VERTEX_POINT('',#4277);
#1375=VERTEX_POINT('',#4281);
#1376=VERTEX_POINT('',#4284);
#1377=VERTEX_POINT('',#4287);
#1378=VERTEX_POINT('',#4291);
#1379=VERTEX_POINT('',#4293);
#1380=VERTEX_POINT('',#4296);
#1381=VERTEX_POINT('',#4305);
#1382=VERTEX_POINT('',#4307);
#1383=VERTEX_POINT('',#4311);
#1384=VERTEX_POINT('',#4314);
#1385=VERTEX_POINT('',#4317);
#1386=VERTEX_POINT('',#4321);
#1387=VERTEX_POINT('',#4323);
#1388=VERTEX_POINT('',#4326);
#1389=VERTEX_POINT('',#4335);
#1390=VERTEX_POINT('',#4337);
#1391=VERTEX_POINT('',#4341);
#1392=VERTEX_POINT('',#4344);
#1393=VERTEX_POINT('',#4347);
#1394=VERTEX_POINT('',#4351);
#1395=VERTEX_POINT('',#4353);
#1396=VERTEX_POINT('',#4356);
#1397=VERTEX_POINT('',#4365);
#1398=VERTEX_POINT('',#4366);
#1399=VERTEX_POINT('',#4368);
#1400=VERTEX_POINT('',#4370);
#1401=VERTEX_POINT('',#4374);
#1402=VERTEX_POINT('',#4375);
#1403=VERTEX_POINT('',#4377);
#1404=VERTEX_POINT('',#4379);
#1405=VERTEX_POINT('',#4392);
#1406=VERTEX_POINT('',#4394);
#1407=VERTEX_POINT('',#4398);
#1408=VERTEX_POINT('',#4399);
#1409=VERTEX_POINT('',#4401);
#1410=VERTEX_POINT('',#4403);
#1411=VERTEX_POINT('',#4407);
#1412=VERTEX_POINT('',#4409);
#1413=VERTEX_POINT('',#4413);
#1414=VERTEX_POINT('',#4415);
#1415=VERTEX_POINT('',#4419);
#1416=VERTEX_POINT('',#4421);
#1417=VERTEX_POINT('',#4425);
#1418=VERTEX_POINT('',#4427);
#1419=VERTEX_POINT('',#4431);
#1420=VERTEX_POINT('',#4433);
#1421=VERTEX_POINT('',#4437);
#1422=VERTEX_POINT('',#4439);
#1423=VERTEX_POINT('',#4443);
#1424=VERTEX_POINT('',#4445);
#1425=VERTEX_POINT('',#4449);
#1426=VERTEX_POINT('',#4451);
#1427=VERTEX_POINT('',#4455);
#1428=VERTEX_POINT('',#4457);
#1429=VERTEX_POINT('',#4461);
#1430=VERTEX_POINT('',#4463);
#1431=VERTEX_POINT('',#4467);
#1432=VERTEX_POINT('',#4469);
#1433=VERTEX_POINT('',#4473);
#1434=VERTEX_POINT('',#4475);
#1435=VERTEX_POINT('',#4479);
#1436=VERTEX_POINT('',#4481);
#1437=VERTEX_POINT('',#4491);
#1438=VERTEX_POINT('',#4493);
#1439=VERTEX_POINT('',#4497);
#1440=VERTEX_POINT('',#4499);
#1441=VERTEX_POINT('',#4506);
#1442=VERTEX_POINT('',#4508);
#1443=VERTEX_POINT('',#4512);
#1444=VERTEX_POINT('',#4514);
#1445=VERTEX_POINT('',#4521);
#1446=VERTEX_POINT('',#4523);
#1447=VERTEX_POINT('',#4527);
#1448=VERTEX_POINT('',#4529);
#1449=VERTEX_POINT('',#4536);
#1450=VERTEX_POINT('',#4538);
#1451=VERTEX_POINT('',#4542);
#1452=VERTEX_POINT('',#4544);
#1453=VERTEX_POINT('',#4551);
#1454=VERTEX_POINT('',#4553);
#1455=VERTEX_POINT('',#4557);
#1456=VERTEX_POINT('',#4559);
#1457=VERTEX_POINT('',#4566);
#1458=VERTEX_POINT('',#4567);
#1459=VERTEX_POINT('',#4569);
#1460=VERTEX_POINT('',#4571);
#1461=VERTEX_POINT('',#4575);
#1462=VERTEX_POINT('',#4576);
#1463=VERTEX_POINT('',#4578);
#1464=VERTEX_POINT('',#4580);
#1465=EDGE_CURVE('',#1241,#1241,#1167,.T.);
#1466=EDGE_CURVE('',#1241,#1242,#643,.T.);
#1467=EDGE_CURVE('',#1242,#1242,#1168,.T.);
#1468=EDGE_CURVE('',#1243,#1243,#1169,.T.);
#1469=EDGE_CURVE('',#1243,#1244,#644,.T.);
#1470=EDGE_CURVE('',#1244,#1244,#1170,.T.);
#1471=EDGE_CURVE('',#1245,#1245,#1171,.F.);
#1472=EDGE_CURVE('',#1245,#1246,#645,.T.);
#1473=EDGE_CURVE('',#1246,#1246,#1172,.T.);
#1474=EDGE_CURVE('',#1247,#1247,#1173,.F.);
#1475=EDGE_CURVE('',#1247,#1248,#646,.T.);
#1476=EDGE_CURVE('',#1248,#1248,#1174,.T.);
#1477=EDGE_CURVE('',#1249,#1249,#1175,.F.);
#1478=EDGE_CURVE('',#1249,#1250,#647,.T.);
#1479=EDGE_CURVE('',#1250,#1250,#1176,.T.);
#1480=EDGE_CURVE('',#1251,#1251,#1177,.F.);
#1481=EDGE_CURVE('',#1251,#1252,#648,.T.);
#1482=EDGE_CURVE('',#1252,#1252,#1178,.T.);
#1483=EDGE_CURVE('',#1253,#1254,#649,.T.);
#1484=EDGE_CURVE('',#1255,#1254,#650,.T.);
#1485=EDGE_CURVE('',#1255,#1256,#651,.T.);
#1486=EDGE_CURVE('',#1256,#1253,#652,.T.);
#1487=EDGE_CURVE('',#1257,#1258,#653,.T.);
#1488=EDGE_CURVE('',#1257,#1259,#654,.T.);
#1489=EDGE_CURVE('',#1260,#1259,#655,.T.);
#1490=EDGE_CURVE('',#1258,#1260,#656,.T.);
#1491=EDGE_CURVE('',#1261,#1262,#657,.T.);
#1492=EDGE_CURVE('',#1262,#1263,#658,.T.);
#1493=EDGE_CURVE('',#1264,#1263,#659,.F.);
#1494=EDGE_CURVE('',#1261,#1264,#660,.F.);
#1495=EDGE_CURVE('',#1259,#1264,#661,.T.);
#1496=EDGE_CURVE('',#1263,#1260,#662,.T.);
#1497=EDGE_CURVE('',#1256,#1261,#663,.T.);
#1498=EDGE_CURVE('',#1262,#1255,#664,.T.);
#1499=EDGE_CURVE('',#1265,#1266,#665,.F.);
#1500=EDGE_CURVE('',#1266,#1267,#666,.T.);
#1501=EDGE_CURVE('',#1268,#1267,#667,.F.);
#1502=EDGE_CURVE('',#1265,#1268,#668,.F.);
#1503=EDGE_CURVE('',#1254,#1265,#669,.T.);
#1504=EDGE_CURVE('',#1258,#1268,#670,.T.);
#1505=EDGE_CURVE('',#1266,#1253,#671,.T.);
#1506=EDGE_CURVE('',#1267,#1257,#672,.T.);
#1507=EDGE_CURVE('',#1269,#1269,#1179,.T.);
#1508=EDGE_CURVE('',#1269,#1270,#673,.T.);
#1509=EDGE_CURVE('',#1270,#1270,#1180,.T.);
#1510=EDGE_CURVE('',#1271,#1272,#674,.T.);
#1511=EDGE_CURVE('',#1272,#1273,#675,.T.);
#1512=EDGE_CURVE('',#1274,#1273,#676,.T.);
#1513=EDGE_CURVE('',#1271,#1274,#677,.T.);
#1514=EDGE_CURVE('',#1275,#1271,#678,.T.);
#1515=EDGE_CURVE('',#1276,#1274,#679,.T.);
#1516=EDGE_CURVE('',#1275,#1276,#680,.T.);
#1517=EDGE_CURVE('',#1277,#1275,#681,.T.);
#1518=EDGE_CURVE('',#1278,#1276,#682,.T.);
#1519=EDGE_CURVE('',#1277,#1278,#683,.T.);
#1520=EDGE_CURVE('',#1279,#1277,#684,.T.);
#1521=EDGE_CURVE('',#1280,#1278,#685,.T.);
#1522=EDGE_CURVE('',#1279,#1280,#686,.T.);
#1523=EDGE_CURVE('',#1281,#1279,#687,.T.);
#1524=EDGE_CURVE('',#1282,#1280,#688,.T.);
#1525=EDGE_CURVE('',#1281,#1282,#689,.T.);
#1526=EDGE_CURVE('',#1283,#1281,#690,.T.);
#1527=EDGE_CURVE('',#1284,#1282,#691,.T.);
#1528=EDGE_CURVE('',#1283,#1284,#692,.T.);
#1529=EDGE_CURVE('',#1285,#1283,#693,.T.);
#1530=EDGE_CURVE('',#1286,#1284,#694,.T.);
#1531=EDGE_CURVE('',#1285,#1286,#695,.T.);
#1532=EDGE_CURVE('',#1287,#1285,#696,.T.);
#1533=EDGE_CURVE('',#1288,#1286,#697,.T.);
#1534=EDGE_CURVE('',#1287,#1288,#698,.T.);
#1535=EDGE_CURVE('',#1289,#1287,#699,.T.);
#1536=EDGE_CURVE('',#1290,#1288,#700,.T.);
#1537=EDGE_CURVE('',#1289,#1290,#701,.T.);
#1538=EDGE_CURVE('',#1291,#1289,#702,.T.);
#1539=EDGE_CURVE('',#1292,#1290,#703,.T.);
#1540=EDGE_CURVE('',#1291,#1292,#704,.T.);
#1541=EDGE_CURVE('',#1293,#1291,#705,.T.);
#1542=EDGE_CURVE('',#1294,#1292,#706,.T.);
#1543=EDGE_CURVE('',#1293,#1294,#707,.T.);
#1544=EDGE_CURVE('',#1295,#1293,#708,.T.);
#1545=EDGE_CURVE('',#1296,#1294,#709,.T.);
#1546=EDGE_CURVE('',#1295,#1296,#710,.T.);
#1547=EDGE_CURVE('',#1297,#1295,#711,.T.);
#1548=EDGE_CURVE('',#1298,#1296,#712,.T.);
#1549=EDGE_CURVE('',#1297,#1298,#713,.T.);
#1550=EDGE_CURVE('',#1299,#1297,#714,.T.);
#1551=EDGE_CURVE('',#1300,#1298,#715,.T.);
#1552=EDGE_CURVE('',#1299,#1300,#716,.T.);
#1553=EDGE_CURVE('',#1301,#1299,#717,.T.);
#1554=EDGE_CURVE('',#1302,#1300,#718,.T.);
#1555=EDGE_CURVE('',#1301,#1302,#719,.T.);
#1556=EDGE_CURVE('',#1303,#1301,#720,.T.);
#1557=EDGE_CURVE('',#1304,#1302,#721,.T.);
#1558=EDGE_CURVE('',#1303,#1304,#722,.T.);
#1559=EDGE_CURVE('',#1305,#1303,#723,.T.);
#1560=EDGE_CURVE('',#1306,#1304,#724,.T.);
#1561=EDGE_CURVE('',#1305,#1306,#725,.T.);
#1562=EDGE_CURVE('',#1307,#1305,#726,.T.);
#1563=EDGE_CURVE('',#1308,#1306,#727,.T.);
#1564=EDGE_CURVE('',#1307,#1308,#728,.T.);
#1565=EDGE_CURVE('',#1309,#1307,#729,.T.);
#1566=EDGE_CURVE('',#1310,#1308,#730,.T.);
#1567=EDGE_CURVE('',#1309,#1310,#731,.T.);
#1568=EDGE_CURVE('',#1311,#1309,#732,.T.);
#1569=EDGE_CURVE('',#1312,#1310,#733,.T.);
#1570=EDGE_CURVE('',#1311,#1312,#734,.T.);
#1571=EDGE_CURVE('',#1313,#1311,#735,.T.);
#1572=EDGE_CURVE('',#1314,#1312,#736,.T.);
#1573=EDGE_CURVE('',#1313,#1314,#737,.T.);
#1574=EDGE_CURVE('',#1315,#1313,#738,.T.);
#1575=EDGE_CURVE('',#1316,#1314,#739,.T.);
#1576=EDGE_CURVE('',#1315,#1316,#740,.T.);
#1577=EDGE_CURVE('',#1317,#1315,#741,.T.);
#1578=EDGE_CURVE('',#1318,#1316,#742,.T.);
#1579=EDGE_CURVE('',#1317,#1318,#743,.T.);
#1580=EDGE_CURVE('',#1319,#1317,#744,.T.);
#1581=EDGE_CURVE('',#1320,#1318,#745,.T.);
#1582=EDGE_CURVE('',#1319,#1320,#746,.T.);
#1583=EDGE_CURVE('',#1321,#1319,#747,.T.);
#1584=EDGE_CURVE('',#1322,#1320,#748,.T.);
#1585=EDGE_CURVE('',#1321,#1322,#749,.T.);
#1586=EDGE_CURVE('',#1323,#1321,#750,.T.);
#1587=EDGE_CURVE('',#1324,#1322,#751,.T.);
#1588=EDGE_CURVE('',#1323,#1324,#752,.T.);
#1589=EDGE_CURVE('',#1325,#1323,#753,.T.);
#1590=EDGE_CURVE('',#1326,#1324,#754,.T.);
#1591=EDGE_CURVE('',#1325,#1326,#755,.T.);
#1592=EDGE_CURVE('',#1327,#1325,#756,.T.);
#1593=EDGE_CURVE('',#1328,#1326,#757,.T.);
#1594=EDGE_CURVE('',#1327,#1328,#758,.T.);
#1595=EDGE_CURVE('',#1329,#1327,#759,.T.);
#1596=EDGE_CURVE('',#1330,#1328,#760,.T.);
#1597=EDGE_CURVE('',#1329,#1330,#761,.T.);
#1598=EDGE_CURVE('',#1331,#1329,#762,.T.);
#1599=EDGE_CURVE('',#1332,#1330,#763,.T.);
#1600=EDGE_CURVE('',#1331,#1332,#764,.T.);
#1601=EDGE_CURVE('',#1333,#1331,#765,.T.);
#1602=EDGE_CURVE('',#1334,#1332,#766,.T.);
#1603=EDGE_CURVE('',#1333,#1334,#767,.T.);
#1604=EDGE_CURVE('',#1335,#1333,#768,.T.);
#1605=EDGE_CURVE('',#1336,#1334,#769,.T.);
#1606=EDGE_CURVE('',#1335,#1336,#770,.T.);
#1607=EDGE_CURVE('',#1337,#1335,#771,.T.);
#1608=EDGE_CURVE('',#1338,#1336,#772,.T.);
#1609=EDGE_CURVE('',#1337,#1338,#773,.T.);
#1610=EDGE_CURVE('',#1339,#1337,#774,.T.);
#1611=EDGE_CURVE('',#1340,#1338,#775,.T.);
#1612=EDGE_CURVE('',#1339,#1340,#776,.T.);
#1613=EDGE_CURVE('',#1341,#1339,#777,.T.);
#1614=EDGE_CURVE('',#1342,#1340,#778,.T.);
#1615=EDGE_CURVE('',#1341,#1342,#779,.T.);
#1616=EDGE_CURVE('',#1343,#1341,#780,.T.);
#1617=EDGE_CURVE('',#1344,#1342,#781,.T.);
#1618=EDGE_CURVE('',#1343,#1344,#782,.T.);
#1619=EDGE_CURVE('',#1345,#1343,#783,.T.);
#1620=EDGE_CURVE('',#1346,#1344,#784,.T.);
#1621=EDGE_CURVE('',#1345,#1346,#785,.T.);
#1622=EDGE_CURVE('',#1347,#1345,#786,.T.);
#1623=EDGE_CURVE('',#1348,#1346,#787,.T.);
#1624=EDGE_CURVE('',#1347,#1348,#788,.T.);
#1625=EDGE_CURVE('',#1349,#1347,#789,.T.);
#1626=EDGE_CURVE('',#1350,#1348,#790,.T.);
#1627=EDGE_CURVE('',#1349,#1350,#791,.T.);
#1628=EDGE_CURVE('',#1272,#1349,#792,.T.);
#1629=EDGE_CURVE('',#1273,#1350,#793,.T.);
#1630=EDGE_CURVE('',#1351,#1351,#1181,.T.);
#1631=EDGE_CURVE('',#1351,#1352,#794,.T.);
#1632=EDGE_CURVE('',#1352,#1352,#1182,.T.);
#1633=EDGE_CURVE('',#1353,#1353,#1183,.T.);
#1634=EDGE_CURVE('',#1353,#1354,#795,.T.);
#1635=EDGE_CURVE('',#1354,#1354,#1184,.T.);
#1636=EDGE_CURVE('',#1355,#1355,#1185,.T.);
#1637=EDGE_CURVE('',#1355,#1356,#796,.T.);
#1638=EDGE_CURVE('',#1356,#1356,#1186,.T.);
#1639=EDGE_CURVE('',#1357,#1358,#797,.T.);
#1640=EDGE_CURVE('',#1358,#1359,#798,.T.);
#1641=EDGE_CURVE('',#1360,#1359,#799,.T.);
#1642=EDGE_CURVE('',#1357,#1360,#800,.T.);
#1643=EDGE_CURVE('',#1361,#1357,#801,.T.);
#1644=EDGE_CURVE('',#1362,#1360,#802,.T.);
#1645=EDGE_CURVE('',#1361,#1362,#803,.T.);
#1646=EDGE_CURVE('',#1363,#1361,#804,.T.);
#1647=EDGE_CURVE('',#1364,#1362,#805,.T.);
#1648=EDGE_CURVE('',#1363,#1364,#806,.T.);
#1649=EDGE_CURVE('',#1365,#1363,#807,.T.);
#1650=EDGE_CURVE('',#1366,#1364,#808,.T.);
#1651=EDGE_CURVE('',#1365,#1366,#809,.T.);
#1652=EDGE_CURVE('',#1367,#1365,#810,.T.);
#1653=EDGE_CURVE('',#1368,#1366,#811,.T.);
#1654=EDGE_CURVE('',#1367,#1368,#812,.T.);
#1655=EDGE_CURVE('',#1369,#1367,#813,.T.);
#1656=EDGE_CURVE('',#1370,#1368,#814,.T.);
#1657=EDGE_CURVE('',#1369,#1370,#815,.T.);
#1658=EDGE_CURVE('',#1371,#1369,#816,.T.);
#1659=EDGE_CURVE('',#1372,#1370,#817,.T.);
#1660=EDGE_CURVE('',#1371,#1372,#818,.T.);
#1661=EDGE_CURVE('',#1358,#1371,#819,.T.);
#1662=EDGE_CURVE('',#1359,#1372,#820,.T.);
#1663=EDGE_CURVE('',#1373,#1373,#1187,.T.);
#1664=EDGE_CURVE('',#1373,#1374,#821,.T.);
#1665=EDGE_CURVE('',#1374,#1374,#1188,.T.);
#1666=EDGE_CURVE('',#1375,#1375,#1189,.T.);
#1667=EDGE_CURVE('',#1376,#1376,#1190,.T.);
#1668=EDGE_CURVE('',#1377,#1377,#1191,.T.);
#1669=EDGE_CURVE('',#1377,#1376,#822,.T.);
#1670=EDGE_CURVE('',#1378,#1378,#1192,.T.);
#1671=EDGE_CURVE('',#1379,#1379,#1193,.T.);
#1672=EDGE_CURVE('',#1378,#1380,#823,.T.);
#1673=EDGE_CURVE('',#1380,#1380,#1194,.T.);
#1674=EDGE_CURVE('',#1375,#1379,#824,.T.);
#1675=EDGE_CURVE('',#1381,#1381,#1195,.T.);
#1676=EDGE_CURVE('',#1381,#1382,#825,.T.);
#1677=EDGE_CURVE('',#1382,#1382,#1196,.T.);
#1678=EDGE_CURVE('',#1383,#1383,#1197,.T.);
#1679=EDGE_CURVE('',#1384,#1384,#1198,.T.);
#1680=EDGE_CURVE('',#1385,#1385,#1199,.T.);
#1681=EDGE_CURVE('',#1385,#1384,#826,.T.);
#1682=EDGE_CURVE('',#1386,#1386,#1200,.T.);
#1683=EDGE_CURVE('',#1387,#1387,#1201,.T.);
#1684=EDGE_CURVE('',#1386,#1388,#827,.T.);
#1685=EDGE_CURVE('',#1388,#1388,#1202,.T.);
#1686=EDGE_CURVE('',#1383,#1387,#828,.T.);
#1687=EDGE_CURVE('',#1389,#1389,#1203,.T.);
#1688=EDGE_CURVE('',#1389,#1390,#829,.T.);
#1689=EDGE_CURVE('',#1390,#1390,#1204,.T.);
#1690=EDGE_CURVE('',#1391,#1391,#1205,.T.);
#1691=EDGE_CURVE('',#1392,#1392,#1206,.T.);
#1692=EDGE_CURVE('',#1393,#1393,#1207,.T.);
#1693=EDGE_CURVE('',#1393,#1392,#830,.T.);
#1694=EDGE_CURVE('',#1394,#1394,#1208,.T.);
#1695=EDGE_CURVE('',#1395,#1395,#1209,.T.);
#1696=EDGE_CURVE('',#1394,#1396,#831,.T.);
#1697=EDGE_CURVE('',#1396,#1396,#1210,.T.);
#1698=EDGE_CURVE('',#1391,#1395,#832,.T.);
#1699=EDGE_CURVE('',#1397,#1398,#833,.T.);
#1700=EDGE_CURVE('',#1399,#1397,#834,.T.);
#1701=EDGE_CURVE('',#1400,#1399,#835,.T.);
#1702=EDGE_CURVE('',#1398,#1400,#836,.T.);
#1703=EDGE_CURVE('',#1401,#1402,#837,.T.);
#1704=EDGE_CURVE('',#1403,#1401,#838,.T.);
#1705=EDGE_CURVE('',#1404,#1403,#839,.T.);
#1706=EDGE_CURVE('',#1402,#1404,#840,.T.);
#1707=EDGE_CURVE('',#1399,#1404,#1211,.T.);
#1708=EDGE_CURVE('',#1402,#1397,#1212,.T.);
#1709=EDGE_CURVE('',#1401,#1398,#1213,.T.);
#1710=EDGE_CURVE('',#1400,#1403,#1214,.T.);
#1711=EDGE_CURVE('',#1405,#1405,#1215,.T.);
#1712=EDGE_CURVE('',#1405,#1406,#841,.T.);
#1713=EDGE_CURVE('',#1406,#1406,#1216,.T.);
#1714=EDGE_CURVE('',#1407,#1408,#842,.T.);
#1715=EDGE_CURVE('',#1408,#1409,#843,.T.);
#1716=EDGE_CURVE('',#1410,#1409,#844,.T.);
#1717=EDGE_CURVE('',#1407,#1410,#845,.T.);
#1718=EDGE_CURVE('',#1411,#1407,#846,.T.);
#1719=EDGE_CURVE('',#1412,#1410,#847,.T.);
#1720=EDGE_CURVE('',#1411,#1412,#848,.T.);
#1721=EDGE_CURVE('',#1413,#1411,#849,.T.);
#1722=EDGE_CURVE('',#1414,#1412,#850,.T.);
#1723=EDGE_CURVE('',#1413,#1414,#851,.T.);
#1724=EDGE_CURVE('',#1415,#1413,#852,.T.);
#1725=EDGE_CURVE('',#1416,#1414,#853,.T.);
#1726=EDGE_CURVE('',#1415,#1416,#854,.T.);
#1727=EDGE_CURVE('',#1417,#1415,#855,.T.);
#1728=EDGE_CURVE('',#1418,#1416,#856,.T.);
#1729=EDGE_CURVE('',#1417,#1418,#857,.T.);
#1730=EDGE_CURVE('',#1419,#1417,#858,.T.);
#1731=EDGE_CURVE('',#1420,#1418,#859,.T.);
#1732=EDGE_CURVE('',#1419,#1420,#860,.T.);
#1733=EDGE_CURVE('',#1421,#1419,#861,.T.);
#1734=EDGE_CURVE('',#1422,#1420,#862,.T.);
#1735=EDGE_CURVE('',#1421,#1422,#863,.T.);
#1736=EDGE_CURVE('',#1423,#1421,#864,.T.);
#1737=EDGE_CURVE('',#1424,#1422,#865,.T.);
#1738=EDGE_CURVE('',#1423,#1424,#866,.T.);
#1739=EDGE_CURVE('',#1425,#1423,#867,.T.);
#1740=EDGE_CURVE('',#1426,#1424,#868,.T.);
#1741=EDGE_CURVE('',#1425,#1426,#869,.T.);
#1742=EDGE_CURVE('',#1427,#1425,#870,.T.);
#1743=EDGE_CURVE('',#1428,#1426,#871,.T.);
#1744=EDGE_CURVE('',#1427,#1428,#872,.T.);
#1745=EDGE_CURVE('',#1429,#1427,#873,.T.);
#1746=EDGE_CURVE('',#1430,#1428,#874,.T.);
#1747=EDGE_CURVE('',#1429,#1430,#875,.T.);
#1748=EDGE_CURVE('',#1431,#1429,#876,.T.);
#1749=EDGE_CURVE('',#1432,#1430,#877,.T.);
#1750=EDGE_CURVE('',#1431,#1432,#878,.T.);
#1751=EDGE_CURVE('',#1433,#1431,#879,.T.);
#1752=EDGE_CURVE('',#1434,#1432,#880,.T.);
#1753=EDGE_CURVE('',#1433,#1434,#881,.T.);
#1754=EDGE_CURVE('',#1435,#1433,#882,.T.);
#1755=EDGE_CURVE('',#1436,#1434,#883,.T.);
#1756=EDGE_CURVE('',#1435,#1436,#884,.T.);
#1757=EDGE_CURVE('',#1408,#1435,#885,.T.);
#1758=EDGE_CURVE('',#1409,#1436,#886,.T.);
#1759=EDGE_CURVE('',#1437,#1437,#1217,.T.);
#1760=EDGE_CURVE('',#1437,#1438,#887,.T.);
#1761=EDGE_CURVE('',#1438,#1438,#1218,.T.);
#1762=EDGE_CURVE('',#1439,#1439,#1219,.T.);
#1763=EDGE_CURVE('',#1439,#1440,#888,.T.);
#1764=EDGE_CURVE('',#1440,#1440,#1220,.T.);
#1765=EDGE_CURVE('',#1441,#1441,#1221,.T.);
#1766=EDGE_CURVE('',#1441,#1442,#889,.T.);
#1767=EDGE_CURVE('',#1442,#1442,#1222,.T.);
#1768=EDGE_CURVE('',#1443,#1443,#1223,.T.);
#1769=EDGE_CURVE('',#1443,#1444,#890,.T.);
#1770=EDGE_CURVE('',#1444,#1444,#1224,.T.);
#1771=EDGE_CURVE('',#1445,#1445,#1225,.T.);
#1772=EDGE_CURVE('',#1445,#1446,#891,.T.);
#1773=EDGE_CURVE('',#1446,#1446,#1226,.T.);
#1774=EDGE_CURVE('',#1447,#1447,#1227,.T.);
#1775=EDGE_CURVE('',#1447,#1448,#892,.T.);
#1776=EDGE_CURVE('',#1448,#1448,#1228,.T.);
#1777=EDGE_CURVE('',#1449,#1449,#1229,.T.);
#1778=EDGE_CURVE('',#1449,#1450,#893,.T.);
#1779=EDGE_CURVE('',#1450,#1450,#1230,.T.);
#1780=EDGE_CURVE('',#1451,#1451,#1231,.T.);
#1781=EDGE_CURVE('',#1451,#1452,#894,.T.);
#1782=EDGE_CURVE('',#1452,#1452,#1232,.T.);
#1783=EDGE_CURVE('',#1453,#1453,#1233,.T.);
#1784=EDGE_CURVE('',#1453,#1454,#895,.T.);
#1785=EDGE_CURVE('',#1454,#1454,#1234,.T.);
#1786=EDGE_CURVE('',#1455,#1455,#1235,.T.);
#1787=EDGE_CURVE('',#1455,#1456,#896,.T.);
#1788=EDGE_CURVE('',#1456,#1456,#1236,.T.);
#1789=EDGE_CURVE('',#1457,#1458,#897,.T.);
#1790=EDGE_CURVE('',#1459,#1457,#898,.T.);
#1791=EDGE_CURVE('',#1460,#1459,#899,.T.);
#1792=EDGE_CURVE('',#1458,#1460,#900,.T.);
#1793=EDGE_CURVE('',#1461,#1462,#901,.T.);
#1794=EDGE_CURVE('',#1463,#1461,#902,.T.);
#1795=EDGE_CURVE('',#1464,#1463,#903,.T.);
#1796=EDGE_CURVE('',#1462,#1464,#904,.T.);
#1797=EDGE_CURVE('',#1459,#1464,#1237,.T.);
#1798=EDGE_CURVE('',#1462,#1457,#1238,.T.);
#1799=EDGE_CURVE('',#1461,#1458,#1239,.T.);
#1800=EDGE_CURVE('',#1460,#1463,#1240,.T.);
#1801=ORIENTED_EDGE('',*,*,#1465,.F.);
#1802=ORIENTED_EDGE('',*,*,#1466,.T.);
#1803=ORIENTED_EDGE('',*,*,#1467,.F.);
#1804=ORIENTED_EDGE('',*,*,#1466,.F.);
#1805=ORIENTED_EDGE('',*,*,#1468,.F.);
#1806=ORIENTED_EDGE('',*,*,#1469,.T.);
#1807=ORIENTED_EDGE('',*,*,#1470,.F.);
#1808=ORIENTED_EDGE('',*,*,#1469,.F.);
#1809=ORIENTED_EDGE('',*,*,#1471,.F.);
#1810=ORIENTED_EDGE('',*,*,#1472,.T.);
#1811=ORIENTED_EDGE('',*,*,#1473,.F.);
#1812=ORIENTED_EDGE('',*,*,#1472,.F.);
#1813=ORIENTED_EDGE('',*,*,#1474,.F.);
#1814=ORIENTED_EDGE('',*,*,#1475,.T.);
#1815=ORIENTED_EDGE('',*,*,#1476,.F.);
#1816=ORIENTED_EDGE('',*,*,#1475,.F.);
#1817=ORIENTED_EDGE('',*,*,#1477,.F.);
#1818=ORIENTED_EDGE('',*,*,#1478,.T.);
#1819=ORIENTED_EDGE('',*,*,#1479,.F.);
#1820=ORIENTED_EDGE('',*,*,#1478,.F.);
#1821=ORIENTED_EDGE('',*,*,#1480,.F.);
#1822=ORIENTED_EDGE('',*,*,#1481,.T.);
#1823=ORIENTED_EDGE('',*,*,#1482,.F.);
#1824=ORIENTED_EDGE('',*,*,#1481,.F.);
#1825=ORIENTED_EDGE('',*,*,#1483,.T.);
#1826=ORIENTED_EDGE('',*,*,#1484,.F.);
#1827=ORIENTED_EDGE('',*,*,#1485,.T.);
#1828=ORIENTED_EDGE('',*,*,#1486,.T.);
#1829=ORIENTED_EDGE('',*,*,#1473,.T.);
#1830=ORIENTED_EDGE('',*,*,#1476,.T.);
#1831=ORIENTED_EDGE('',*,*,#1487,.F.);
#1832=ORIENTED_EDGE('',*,*,#1488,.T.);
#1833=ORIENTED_EDGE('',*,*,#1489,.F.);
#1834=ORIENTED_EDGE('',*,*,#1490,.F.);
#1835=ORIENTED_EDGE('',*,*,#1479,.T.);
#1836=ORIENTED_EDGE('',*,*,#1482,.T.);
#1837=ORIENTED_EDGE('',*,*,#1491,.T.);
#1838=ORIENTED_EDGE('',*,*,#1492,.T.);
#1839=ORIENTED_EDGE('',*,*,#1493,.F.);
#1840=ORIENTED_EDGE('',*,*,#1494,.F.);
#1841=ORIENTED_EDGE('',*,*,#1471,.T.);
#1842=ORIENTED_EDGE('',*,*,#1474,.T.);
#1843=ORIENTED_EDGE('',*,*,#1477,.T.);
#1844=ORIENTED_EDGE('',*,*,#1480,.T.);
#1845=ORIENTED_EDGE('',*,*,#1495,.T.);
#1846=ORIENTED_EDGE('',*,*,#1493,.T.);
#1847=ORIENTED_EDGE('',*,*,#1496,.T.);
#1848=ORIENTED_EDGE('',*,*,#1489,.T.);
#1849=ORIENTED_EDGE('',*,*,#1497,.F.);
#1850=ORIENTED_EDGE('',*,*,#1485,.F.);
#1851=ORIENTED_EDGE('',*,*,#1498,.F.);
#1852=ORIENTED_EDGE('',*,*,#1491,.F.);
#1853=ORIENTED_EDGE('',*,*,#1499,.T.);
#1854=ORIENTED_EDGE('',*,*,#1500,.T.);
#1855=ORIENTED_EDGE('',*,*,#1501,.F.);
#1856=ORIENTED_EDGE('',*,*,#1502,.F.);
#1857=ORIENTED_EDGE('',*,*,#1503,.T.);
#1858=ORIENTED_EDGE('',*,*,#1502,.T.);
#1859=ORIENTED_EDGE('',*,*,#1504,.F.);
#1860=ORIENTED_EDGE('',*,*,#1490,.T.);
#1861=ORIENTED_EDGE('',*,*,#1496,.F.);
#1862=ORIENTED_EDGE('',*,*,#1492,.F.);
#1863=ORIENTED_EDGE('',*,*,#1498,.T.);
#1864=ORIENTED_EDGE('',*,*,#1484,.T.);
#1865=ORIENTED_EDGE('',*,*,#1505,.T.);
#1866=ORIENTED_EDGE('',*,*,#1486,.F.);
#1867=ORIENTED_EDGE('',*,*,#1497,.T.);
#1868=ORIENTED_EDGE('',*,*,#1494,.T.);
#1869=ORIENTED_EDGE('',*,*,#1495,.F.);
#1870=ORIENTED_EDGE('',*,*,#1488,.F.);
#1871=ORIENTED_EDGE('',*,*,#1506,.F.);
#1872=ORIENTED_EDGE('',*,*,#1500,.F.);
#1873=ORIENTED_EDGE('',*,*,#1506,.T.);
#1874=ORIENTED_EDGE('',*,*,#1487,.T.);
#1875=ORIENTED_EDGE('',*,*,#1504,.T.);
#1876=ORIENTED_EDGE('',*,*,#1501,.T.);
#1877=ORIENTED_EDGE('',*,*,#1465,.T.);
#1878=ORIENTED_EDGE('',*,*,#1468,.T.);
#1879=ORIENTED_EDGE('',*,*,#1505,.F.);
#1880=ORIENTED_EDGE('',*,*,#1499,.F.);
#1881=ORIENTED_EDGE('',*,*,#1503,.F.);
#1882=ORIENTED_EDGE('',*,*,#1483,.F.);
#1883=ORIENTED_EDGE('',*,*,#1467,.T.);
#1884=ORIENTED_EDGE('',*,*,#1470,.T.);
#1885=ORIENTED_EDGE('',*,*,#1507,.F.);
#1886=ORIENTED_EDGE('',*,*,#1508,.T.);
#1887=ORIENTED_EDGE('',*,*,#1509,.F.);
#1888=ORIENTED_EDGE('',*,*,#1508,.F.);
#1889=ORIENTED_EDGE('',*,*,#1510,.T.);
#1890=ORIENTED_EDGE('',*,*,#1511,.T.);
#1891=ORIENTED_EDGE('',*,*,#1512,.F.);
#1892=ORIENTED_EDGE('',*,*,#1513,.F.);
#1893=ORIENTED_EDGE('',*,*,#1514,.T.);
#1894=ORIENTED_EDGE('',*,*,#1513,.T.);
#1895=ORIENTED_EDGE('',*,*,#1515,.F.);
#1896=ORIENTED_EDGE('',*,*,#1516,.F.);
#1897=ORIENTED_EDGE('',*,*,#1517,.T.);
#1898=ORIENTED_EDGE('',*,*,#1516,.T.);
#1899=ORIENTED_EDGE('',*,*,#1518,.F.);
#1900=ORIENTED_EDGE('',*,*,#1519,.F.);
#1901=ORIENTED_EDGE('',*,*,#1520,.T.);
#1902=ORIENTED_EDGE('',*,*,#1519,.T.);
#1903=ORIENTED_EDGE('',*,*,#1521,.F.);
#1904=ORIENTED_EDGE('',*,*,#1522,.F.);
#1905=ORIENTED_EDGE('',*,*,#1523,.T.);
#1906=ORIENTED_EDGE('',*,*,#1522,.T.);
#1907=ORIENTED_EDGE('',*,*,#1524,.F.);
#1908=ORIENTED_EDGE('',*,*,#1525,.F.);
#1909=ORIENTED_EDGE('',*,*,#1526,.T.);
#1910=ORIENTED_EDGE('',*,*,#1525,.T.);
#1911=ORIENTED_EDGE('',*,*,#1527,.F.);
#1912=ORIENTED_EDGE('',*,*,#1528,.F.);
#1913=ORIENTED_EDGE('',*,*,#1529,.T.);
#1914=ORIENTED_EDGE('',*,*,#1528,.T.);
#1915=ORIENTED_EDGE('',*,*,#1530,.F.);
#1916=ORIENTED_EDGE('',*,*,#1531,.F.);
#1917=ORIENTED_EDGE('',*,*,#1532,.T.);
#1918=ORIENTED_EDGE('',*,*,#1531,.T.);
#1919=ORIENTED_EDGE('',*,*,#1533,.F.);
#1920=ORIENTED_EDGE('',*,*,#1534,.F.);
#1921=ORIENTED_EDGE('',*,*,#1535,.T.);
#1922=ORIENTED_EDGE('',*,*,#1534,.T.);
#1923=ORIENTED_EDGE('',*,*,#1536,.F.);
#1924=ORIENTED_EDGE('',*,*,#1537,.F.);
#1925=ORIENTED_EDGE('',*,*,#1538,.T.);
#1926=ORIENTED_EDGE('',*,*,#1537,.T.);
#1927=ORIENTED_EDGE('',*,*,#1539,.F.);
#1928=ORIENTED_EDGE('',*,*,#1540,.F.);
#1929=ORIENTED_EDGE('',*,*,#1541,.T.);
#1930=ORIENTED_EDGE('',*,*,#1540,.T.);
#1931=ORIENTED_EDGE('',*,*,#1542,.F.);
#1932=ORIENTED_EDGE('',*,*,#1543,.F.);
#1933=ORIENTED_EDGE('',*,*,#1544,.T.);
#1934=ORIENTED_EDGE('',*,*,#1543,.T.);
#1935=ORIENTED_EDGE('',*,*,#1545,.F.);
#1936=ORIENTED_EDGE('',*,*,#1546,.F.);
#1937=ORIENTED_EDGE('',*,*,#1547,.T.);
#1938=ORIENTED_EDGE('',*,*,#1546,.T.);
#1939=ORIENTED_EDGE('',*,*,#1548,.F.);
#1940=ORIENTED_EDGE('',*,*,#1549,.F.);
#1941=ORIENTED_EDGE('',*,*,#1550,.T.);
#1942=ORIENTED_EDGE('',*,*,#1549,.T.);
#1943=ORIENTED_EDGE('',*,*,#1551,.F.);
#1944=ORIENTED_EDGE('',*,*,#1552,.F.);
#1945=ORIENTED_EDGE('',*,*,#1553,.T.);
#1946=ORIENTED_EDGE('',*,*,#1552,.T.);
#1947=ORIENTED_EDGE('',*,*,#1554,.F.);
#1948=ORIENTED_EDGE('',*,*,#1555,.F.);
#1949=ORIENTED_EDGE('',*,*,#1556,.T.);
#1950=ORIENTED_EDGE('',*,*,#1555,.T.);
#1951=ORIENTED_EDGE('',*,*,#1557,.F.);
#1952=ORIENTED_EDGE('',*,*,#1558,.F.);
#1953=ORIENTED_EDGE('',*,*,#1559,.T.);
#1954=ORIENTED_EDGE('',*,*,#1558,.T.);
#1955=ORIENTED_EDGE('',*,*,#1560,.F.);
#1956=ORIENTED_EDGE('',*,*,#1561,.F.);
#1957=ORIENTED_EDGE('',*,*,#1562,.T.);
#1958=ORIENTED_EDGE('',*,*,#1561,.T.);
#1959=ORIENTED_EDGE('',*,*,#1563,.F.);
#1960=ORIENTED_EDGE('',*,*,#1564,.F.);
#1961=ORIENTED_EDGE('',*,*,#1565,.T.);
#1962=ORIENTED_EDGE('',*,*,#1564,.T.);
#1963=ORIENTED_EDGE('',*,*,#1566,.F.);
#1964=ORIENTED_EDGE('',*,*,#1567,.F.);
#1965=ORIENTED_EDGE('',*,*,#1568,.T.);
#1966=ORIENTED_EDGE('',*,*,#1567,.T.);
#1967=ORIENTED_EDGE('',*,*,#1569,.F.);
#1968=ORIENTED_EDGE('',*,*,#1570,.F.);
#1969=ORIENTED_EDGE('',*,*,#1571,.T.);
#1970=ORIENTED_EDGE('',*,*,#1570,.T.);
#1971=ORIENTED_EDGE('',*,*,#1572,.F.);
#1972=ORIENTED_EDGE('',*,*,#1573,.F.);
#1973=ORIENTED_EDGE('',*,*,#1574,.T.);
#1974=ORIENTED_EDGE('',*,*,#1573,.T.);
#1975=ORIENTED_EDGE('',*,*,#1575,.F.);
#1976=ORIENTED_EDGE('',*,*,#1576,.F.);
#1977=ORIENTED_EDGE('',*,*,#1577,.T.);
#1978=ORIENTED_EDGE('',*,*,#1576,.T.);
#1979=ORIENTED_EDGE('',*,*,#1578,.F.);
#1980=ORIENTED_EDGE('',*,*,#1579,.F.);
#1981=ORIENTED_EDGE('',*,*,#1580,.T.);
#1982=ORIENTED_EDGE('',*,*,#1579,.T.);
#1983=ORIENTED_EDGE('',*,*,#1581,.F.);
#1984=ORIENTED_EDGE('',*,*,#1582,.F.);
#1985=ORIENTED_EDGE('',*,*,#1583,.T.);
#1986=ORIENTED_EDGE('',*,*,#1582,.T.);
#1987=ORIENTED_EDGE('',*,*,#1584,.F.);
#1988=ORIENTED_EDGE('',*,*,#1585,.F.);
#1989=ORIENTED_EDGE('',*,*,#1586,.T.);
#1990=ORIENTED_EDGE('',*,*,#1585,.T.);
#1991=ORIENTED_EDGE('',*,*,#1587,.F.);
#1992=ORIENTED_EDGE('',*,*,#1588,.F.);
#1993=ORIENTED_EDGE('',*,*,#1589,.T.);
#1994=ORIENTED_EDGE('',*,*,#1588,.T.);
#1995=ORIENTED_EDGE('',*,*,#1590,.F.);
#1996=ORIENTED_EDGE('',*,*,#1591,.F.);
#1997=ORIENTED_EDGE('',*,*,#1592,.T.);
#1998=ORIENTED_EDGE('',*,*,#1591,.T.);
#1999=ORIENTED_EDGE('',*,*,#1593,.F.);
#2000=ORIENTED_EDGE('',*,*,#1594,.F.);
#2001=ORIENTED_EDGE('',*,*,#1595,.T.);
#2002=ORIENTED_EDGE('',*,*,#1594,.T.);
#2003=ORIENTED_EDGE('',*,*,#1596,.F.);
#2004=ORIENTED_EDGE('',*,*,#1597,.F.);
#2005=ORIENTED_EDGE('',*,*,#1598,.T.);
#2006=ORIENTED_EDGE('',*,*,#1597,.T.);
#2007=ORIENTED_EDGE('',*,*,#1599,.F.);
#2008=ORIENTED_EDGE('',*,*,#1600,.F.);
#2009=ORIENTED_EDGE('',*,*,#1601,.T.);
#2010=ORIENTED_EDGE('',*,*,#1600,.T.);
#2011=ORIENTED_EDGE('',*,*,#1602,.F.);
#2012=ORIENTED_EDGE('',*,*,#1603,.F.);
#2013=ORIENTED_EDGE('',*,*,#1604,.T.);
#2014=ORIENTED_EDGE('',*,*,#1603,.T.);
#2015=ORIENTED_EDGE('',*,*,#1605,.F.);
#2016=ORIENTED_EDGE('',*,*,#1606,.F.);
#2017=ORIENTED_EDGE('',*,*,#1607,.T.);
#2018=ORIENTED_EDGE('',*,*,#1606,.T.);
#2019=ORIENTED_EDGE('',*,*,#1608,.F.);
#2020=ORIENTED_EDGE('',*,*,#1609,.F.);
#2021=ORIENTED_EDGE('',*,*,#1610,.T.);
#2022=ORIENTED_EDGE('',*,*,#1609,.T.);
#2023=ORIENTED_EDGE('',*,*,#1611,.F.);
#2024=ORIENTED_EDGE('',*,*,#1612,.F.);
#2025=ORIENTED_EDGE('',*,*,#1613,.T.);
#2026=ORIENTED_EDGE('',*,*,#1612,.T.);
#2027=ORIENTED_EDGE('',*,*,#1614,.F.);
#2028=ORIENTED_EDGE('',*,*,#1615,.F.);
#2029=ORIENTED_EDGE('',*,*,#1616,.T.);
#2030=ORIENTED_EDGE('',*,*,#1615,.T.);
#2031=ORIENTED_EDGE('',*,*,#1617,.F.);
#2032=ORIENTED_EDGE('',*,*,#1618,.F.);
#2033=ORIENTED_EDGE('',*,*,#1619,.T.);
#2034=ORIENTED_EDGE('',*,*,#1618,.T.);
#2035=ORIENTED_EDGE('',*,*,#1620,.F.);
#2036=ORIENTED_EDGE('',*,*,#1621,.F.);
#2037=ORIENTED_EDGE('',*,*,#1622,.T.);
#2038=ORIENTED_EDGE('',*,*,#1621,.T.);
#2039=ORIENTED_EDGE('',*,*,#1623,.F.);
#2040=ORIENTED_EDGE('',*,*,#1624,.F.);
#2041=ORIENTED_EDGE('',*,*,#1625,.T.);
#2042=ORIENTED_EDGE('',*,*,#1624,.T.);
#2043=ORIENTED_EDGE('',*,*,#1626,.F.);
#2044=ORIENTED_EDGE('',*,*,#1627,.F.);
#2045=ORIENTED_EDGE('',*,*,#1628,.T.);
#2046=ORIENTED_EDGE('',*,*,#1627,.T.);
#2047=ORIENTED_EDGE('',*,*,#1629,.F.);
#2048=ORIENTED_EDGE('',*,*,#1511,.F.);
#2049=ORIENTED_EDGE('',*,*,#1629,.T.);
#2050=ORIENTED_EDGE('',*,*,#1626,.T.);
#2051=ORIENTED_EDGE('',*,*,#1623,.T.);
#2052=ORIENTED_EDGE('',*,*,#1620,.T.);
#2053=ORIENTED_EDGE('',*,*,#1617,.T.);
#2054=ORIENTED_EDGE('',*,*,#1614,.T.);
#2055=ORIENTED_EDGE('',*,*,#1611,.T.);
#2056=ORIENTED_EDGE('',*,*,#1608,.T.);
#2057=ORIENTED_EDGE('',*,*,#1605,.T.);
#2058=ORIENTED_EDGE('',*,*,#1602,.T.);
#2059=ORIENTED_EDGE('',*,*,#1599,.T.);
#2060=ORIENTED_EDGE('',*,*,#1596,.T.);
#2061=ORIENTED_EDGE('',*,*,#1593,.T.);
#2062=ORIENTED_EDGE('',*,*,#1590,.T.);
#2063=ORIENTED_EDGE('',*,*,#1587,.T.);
#2064=ORIENTED_EDGE('',*,*,#1584,.T.);
#2065=ORIENTED_EDGE('',*,*,#1581,.T.);
#2066=ORIENTED_EDGE('',*,*,#1578,.T.);
#2067=ORIENTED_EDGE('',*,*,#1575,.T.);
#2068=ORIENTED_EDGE('',*,*,#1572,.T.);
#2069=ORIENTED_EDGE('',*,*,#1569,.T.);
#2070=ORIENTED_EDGE('',*,*,#1566,.T.);
#2071=ORIENTED_EDGE('',*,*,#1563,.T.);
#2072=ORIENTED_EDGE('',*,*,#1560,.T.);
#2073=ORIENTED_EDGE('',*,*,#1557,.T.);
#2074=ORIENTED_EDGE('',*,*,#1554,.T.);
#2075=ORIENTED_EDGE('',*,*,#1551,.T.);
#2076=ORIENTED_EDGE('',*,*,#1548,.T.);
#2077=ORIENTED_EDGE('',*,*,#1545,.T.);
#2078=ORIENTED_EDGE('',*,*,#1542,.T.);
#2079=ORIENTED_EDGE('',*,*,#1539,.T.);
#2080=ORIENTED_EDGE('',*,*,#1536,.T.);
#2081=ORIENTED_EDGE('',*,*,#1533,.T.);
#2082=ORIENTED_EDGE('',*,*,#1530,.T.);
#2083=ORIENTED_EDGE('',*,*,#1527,.T.);
#2084=ORIENTED_EDGE('',*,*,#1524,.T.);
#2085=ORIENTED_EDGE('',*,*,#1521,.T.);
#2086=ORIENTED_EDGE('',*,*,#1518,.T.);
#2087=ORIENTED_EDGE('',*,*,#1515,.T.);
#2088=ORIENTED_EDGE('',*,*,#1512,.T.);
#2089=ORIENTED_EDGE('',*,*,#1507,.T.);
#2090=ORIENTED_EDGE('',*,*,#1628,.F.);
#2091=ORIENTED_EDGE('',*,*,#1510,.F.);
#2092=ORIENTED_EDGE('',*,*,#1514,.F.);
#2093=ORIENTED_EDGE('',*,*,#1517,.F.);
#2094=ORIENTED_EDGE('',*,*,#1520,.F.);
#2095=ORIENTED_EDGE('',*,*,#1523,.F.);
#2096=ORIENTED_EDGE('',*,*,#1526,.F.);
#2097=ORIENTED_EDGE('',*,*,#1529,.F.);
#2098=ORIENTED_EDGE('',*,*,#1532,.F.);
#2099=ORIENTED_EDGE('',*,*,#1535,.F.);
#2100=ORIENTED_EDGE('',*,*,#1538,.F.);
#2101=ORIENTED_EDGE('',*,*,#1541,.F.);
#2102=ORIENTED_EDGE('',*,*,#1544,.F.);
#2103=ORIENTED_EDGE('',*,*,#1547,.F.);
#2104=ORIENTED_EDGE('',*,*,#1550,.F.);
#2105=ORIENTED_EDGE('',*,*,#1553,.F.);
#2106=ORIENTED_EDGE('',*,*,#1556,.F.);
#2107=ORIENTED_EDGE('',*,*,#1559,.F.);
#2108=ORIENTED_EDGE('',*,*,#1562,.F.);
#2109=ORIENTED_EDGE('',*,*,#1565,.F.);
#2110=ORIENTED_EDGE('',*,*,#1568,.F.);
#2111=ORIENTED_EDGE('',*,*,#1571,.F.);
#2112=ORIENTED_EDGE('',*,*,#1574,.F.);
#2113=ORIENTED_EDGE('',*,*,#1577,.F.);
#2114=ORIENTED_EDGE('',*,*,#1580,.F.);
#2115=ORIENTED_EDGE('',*,*,#1583,.F.);
#2116=ORIENTED_EDGE('',*,*,#1586,.F.);
#2117=ORIENTED_EDGE('',*,*,#1589,.F.);
#2118=ORIENTED_EDGE('',*,*,#1592,.F.);
#2119=ORIENTED_EDGE('',*,*,#1595,.F.);
#2120=ORIENTED_EDGE('',*,*,#1598,.F.);
#2121=ORIENTED_EDGE('',*,*,#1601,.F.);
#2122=ORIENTED_EDGE('',*,*,#1604,.F.);
#2123=ORIENTED_EDGE('',*,*,#1607,.F.);
#2124=ORIENTED_EDGE('',*,*,#1610,.F.);
#2125=ORIENTED_EDGE('',*,*,#1613,.F.);
#2126=ORIENTED_EDGE('',*,*,#1616,.F.);
#2127=ORIENTED_EDGE('',*,*,#1619,.F.);
#2128=ORIENTED_EDGE('',*,*,#1622,.F.);
#2129=ORIENTED_EDGE('',*,*,#1625,.F.);
#2130=ORIENTED_EDGE('',*,*,#1509,.T.);
#2131=ORIENTED_EDGE('',*,*,#1630,.F.);
#2132=ORIENTED_EDGE('',*,*,#1631,.T.);
#2133=ORIENTED_EDGE('',*,*,#1632,.F.);
#2134=ORIENTED_EDGE('',*,*,#1631,.F.);
#2135=ORIENTED_EDGE('',*,*,#1633,.F.);
#2136=ORIENTED_EDGE('',*,*,#1634,.T.);
#2137=ORIENTED_EDGE('',*,*,#1635,.F.);
#2138=ORIENTED_EDGE('',*,*,#1634,.F.);
#2139=ORIENTED_EDGE('',*,*,#1636,.F.);
#2140=ORIENTED_EDGE('',*,*,#1637,.T.);
#2141=ORIENTED_EDGE('',*,*,#1638,.F.);
#2142=ORIENTED_EDGE('',*,*,#1637,.F.);
#2143=ORIENTED_EDGE('',*,*,#1639,.T.);
#2144=ORIENTED_EDGE('',*,*,#1640,.T.);
#2145=ORIENTED_EDGE('',*,*,#1641,.F.);
#2146=ORIENTED_EDGE('',*,*,#1642,.F.);
#2147=ORIENTED_EDGE('',*,*,#1643,.T.);
#2148=ORIENTED_EDGE('',*,*,#1642,.T.);
#2149=ORIENTED_EDGE('',*,*,#1644,.F.);
#2150=ORIENTED_EDGE('',*,*,#1645,.F.);
#2151=ORIENTED_EDGE('',*,*,#1646,.T.);
#2152=ORIENTED_EDGE('',*,*,#1645,.T.);
#2153=ORIENTED_EDGE('',*,*,#1647,.F.);
#2154=ORIENTED_EDGE('',*,*,#1648,.F.);
#2155=ORIENTED_EDGE('',*,*,#1649,.T.);
#2156=ORIENTED_EDGE('',*,*,#1648,.T.);
#2157=ORIENTED_EDGE('',*,*,#1650,.F.);
#2158=ORIENTED_EDGE('',*,*,#1651,.F.);
#2159=ORIENTED_EDGE('',*,*,#1652,.T.);
#2160=ORIENTED_EDGE('',*,*,#1651,.T.);
#2161=ORIENTED_EDGE('',*,*,#1653,.F.);
#2162=ORIENTED_EDGE('',*,*,#1654,.F.);
#2163=ORIENTED_EDGE('',*,*,#1655,.T.);
#2164=ORIENTED_EDGE('',*,*,#1654,.T.);
#2165=ORIENTED_EDGE('',*,*,#1656,.F.);
#2166=ORIENTED_EDGE('',*,*,#1657,.F.);
#2167=ORIENTED_EDGE('',*,*,#1658,.T.);
#2168=ORIENTED_EDGE('',*,*,#1657,.T.);
#2169=ORIENTED_EDGE('',*,*,#1659,.F.);
#2170=ORIENTED_EDGE('',*,*,#1660,.F.);
#2171=ORIENTED_EDGE('',*,*,#1661,.T.);
#2172=ORIENTED_EDGE('',*,*,#1660,.T.);
#2173=ORIENTED_EDGE('',*,*,#1662,.F.);
#2174=ORIENTED_EDGE('',*,*,#1640,.F.);
#2175=ORIENTED_EDGE('',*,*,#1662,.T.);
#2176=ORIENTED_EDGE('',*,*,#1659,.T.);
#2177=ORIENTED_EDGE('',*,*,#1656,.T.);
#2178=ORIENTED_EDGE('',*,*,#1653,.T.);
#2179=ORIENTED_EDGE('',*,*,#1650,.T.);
#2180=ORIENTED_EDGE('',*,*,#1647,.T.);
#2181=ORIENTED_EDGE('',*,*,#1644,.T.);
#2182=ORIENTED_EDGE('',*,*,#1641,.T.);
#2183=ORIENTED_EDGE('',*,*,#1630,.T.);
#2184=ORIENTED_EDGE('',*,*,#1633,.T.);
#2185=ORIENTED_EDGE('',*,*,#1636,.T.);
#2186=ORIENTED_EDGE('',*,*,#1661,.F.);
#2187=ORIENTED_EDGE('',*,*,#1639,.F.);
#2188=ORIENTED_EDGE('',*,*,#1643,.F.);
#2189=ORIENTED_EDGE('',*,*,#1646,.F.);
#2190=ORIENTED_EDGE('',*,*,#1649,.F.);
#2191=ORIENTED_EDGE('',*,*,#1652,.F.);
#2192=ORIENTED_EDGE('',*,*,#1655,.F.);
#2193=ORIENTED_EDGE('',*,*,#1658,.F.);
#2194=ORIENTED_EDGE('',*,*,#1632,.T.);
#2195=ORIENTED_EDGE('',*,*,#1635,.T.);
#2196=ORIENTED_EDGE('',*,*,#1638,.T.);
#2197=ORIENTED_EDGE('',*,*,#1663,.T.);
#2198=ORIENTED_EDGE('',*,*,#1664,.T.);
#2199=ORIENTED_EDGE('',*,*,#1665,.F.);
#2200=ORIENTED_EDGE('',*,*,#1664,.F.);
#2201=ORIENTED_EDGE('',*,*,#1666,.F.);
#2202=ORIENTED_EDGE('',*,*,#1663,.F.);
#2203=ORIENTED_EDGE('',*,*,#1667,.F.);
#2204=ORIENTED_EDGE('',*,*,#1665,.T.);
#2205=ORIENTED_EDGE('',*,*,#1668,.F.);
#2206=ORIENTED_EDGE('',*,*,#1669,.T.);
#2207=ORIENTED_EDGE('',*,*,#1667,.T.);
#2208=ORIENTED_EDGE('',*,*,#1669,.F.);
#2209=ORIENTED_EDGE('',*,*,#1670,.T.);
#2210=ORIENTED_EDGE('',*,*,#1671,.F.);
#2211=ORIENTED_EDGE('',*,*,#1670,.F.);
#2212=ORIENTED_EDGE('',*,*,#1672,.T.);
#2213=ORIENTED_EDGE('',*,*,#1673,.T.);
#2214=ORIENTED_EDGE('',*,*,#1672,.F.);
#2215=ORIENTED_EDGE('',*,*,#1673,.F.);
#2216=ORIENTED_EDGE('',*,*,#1666,.T.);
#2217=ORIENTED_EDGE('',*,*,#1674,.T.);
#2218=ORIENTED_EDGE('',*,*,#1671,.T.);
#2219=ORIENTED_EDGE('',*,*,#1674,.F.);
#2220=ORIENTED_EDGE('',*,*,#1668,.T.);
#2221=ORIENTED_EDGE('',*,*,#1675,.T.);
#2222=ORIENTED_EDGE('',*,*,#1676,.T.);
#2223=ORIENTED_EDGE('',*,*,#1677,.F.);
#2224=ORIENTED_EDGE('',*,*,#1676,.F.);
#2225=ORIENTED_EDGE('',*,*,#1678,.F.);
#2226=ORIENTED_EDGE('',*,*,#1675,.F.);
#2227=ORIENTED_EDGE('',*,*,#1679,.F.);
#2228=ORIENTED_EDGE('',*,*,#1677,.T.);
#2229=ORIENTED_EDGE('',*,*,#1680,.F.);
#2230=ORIENTED_EDGE('',*,*,#1681,.T.);
#2231=ORIENTED_EDGE('',*,*,#1679,.T.);
#2232=ORIENTED_EDGE('',*,*,#1681,.F.);
#2233=ORIENTED_EDGE('',*,*,#1682,.T.);
#2234=ORIENTED_EDGE('',*,*,#1683,.F.);
#2235=ORIENTED_EDGE('',*,*,#1682,.F.);
#2236=ORIENTED_EDGE('',*,*,#1684,.T.);
#2237=ORIENTED_EDGE('',*,*,#1685,.T.);
#2238=ORIENTED_EDGE('',*,*,#1684,.F.);
#2239=ORIENTED_EDGE('',*,*,#1685,.F.);
#2240=ORIENTED_EDGE('',*,*,#1678,.T.);
#2241=ORIENTED_EDGE('',*,*,#1686,.T.);
#2242=ORIENTED_EDGE('',*,*,#1683,.T.);
#2243=ORIENTED_EDGE('',*,*,#1686,.F.);
#2244=ORIENTED_EDGE('',*,*,#1680,.T.);
#2245=ORIENTED_EDGE('',*,*,#1687,.T.);
#2246=ORIENTED_EDGE('',*,*,#1688,.T.);
#2247=ORIENTED_EDGE('',*,*,#1689,.F.);
#2248=ORIENTED_EDGE('',*,*,#1688,.F.);
#2249=ORIENTED_EDGE('',*,*,#1690,.F.);
#2250=ORIENTED_EDGE('',*,*,#1687,.F.);
#2251=ORIENTED_EDGE('',*,*,#1691,.F.);
#2252=ORIENTED_EDGE('',*,*,#1689,.T.);
#2253=ORIENTED_EDGE('',*,*,#1692,.F.);
#2254=ORIENTED_EDGE('',*,*,#1693,.T.);
#2255=ORIENTED_EDGE('',*,*,#1691,.T.);
#2256=ORIENTED_EDGE('',*,*,#1693,.F.);
#2257=ORIENTED_EDGE('',*,*,#1694,.T.);
#2258=ORIENTED_EDGE('',*,*,#1695,.F.);
#2259=ORIENTED_EDGE('',*,*,#1694,.F.);
#2260=ORIENTED_EDGE('',*,*,#1696,.T.);
#2261=ORIENTED_EDGE('',*,*,#1697,.T.);
#2262=ORIENTED_EDGE('',*,*,#1696,.F.);
#2263=ORIENTED_EDGE('',*,*,#1697,.F.);
#2264=ORIENTED_EDGE('',*,*,#1690,.T.);
#2265=ORIENTED_EDGE('',*,*,#1698,.T.);
#2266=ORIENTED_EDGE('',*,*,#1695,.T.);
#2267=ORIENTED_EDGE('',*,*,#1698,.F.);
#2268=ORIENTED_EDGE('',*,*,#1692,.T.);
#2269=ORIENTED_EDGE('',*,*,#1699,.F.);
#2270=ORIENTED_EDGE('',*,*,#1700,.F.);
#2271=ORIENTED_EDGE('',*,*,#1701,.F.);
#2272=ORIENTED_EDGE('',*,*,#1702,.F.);
#2273=ORIENTED_EDGE('',*,*,#1703,.F.);
#2274=ORIENTED_EDGE('',*,*,#1704,.F.);
#2275=ORIENTED_EDGE('',*,*,#1705,.F.);
#2276=ORIENTED_EDGE('',*,*,#1706,.F.);
#2277=ORIENTED_EDGE('',*,*,#1706,.T.);
#2278=ORIENTED_EDGE('',*,*,#1707,.F.);
#2279=ORIENTED_EDGE('',*,*,#1700,.T.);
#2280=ORIENTED_EDGE('',*,*,#1708,.F.);
#2281=ORIENTED_EDGE('',*,*,#1703,.T.);
#2282=ORIENTED_EDGE('',*,*,#1708,.T.);
#2283=ORIENTED_EDGE('',*,*,#1699,.T.);
#2284=ORIENTED_EDGE('',*,*,#1709,.F.);
#2285=ORIENTED_EDGE('',*,*,#1705,.T.);
#2286=ORIENTED_EDGE('',*,*,#1710,.F.);
#2287=ORIENTED_EDGE('',*,*,#1701,.T.);
#2288=ORIENTED_EDGE('',*,*,#1707,.T.);
#2289=ORIENTED_EDGE('',*,*,#1704,.T.);
#2290=ORIENTED_EDGE('',*,*,#1709,.T.);
#2291=ORIENTED_EDGE('',*,*,#1702,.T.);
#2292=ORIENTED_EDGE('',*,*,#1710,.T.);
#2293=ORIENTED_EDGE('',*,*,#1711,.F.);
#2294=ORIENTED_EDGE('',*,*,#1712,.T.);
#2295=ORIENTED_EDGE('',*,*,#1713,.F.);
#2296=ORIENTED_EDGE('',*,*,#1712,.F.);
#2297=ORIENTED_EDGE('',*,*,#1714,.T.);
#2298=ORIENTED_EDGE('',*,*,#1715,.T.);
#2299=ORIENTED_EDGE('',*,*,#1716,.F.);
#2300=ORIENTED_EDGE('',*,*,#1717,.F.);
#2301=ORIENTED_EDGE('',*,*,#1718,.T.);
#2302=ORIENTED_EDGE('',*,*,#1717,.T.);
#2303=ORIENTED_EDGE('',*,*,#1719,.F.);
#2304=ORIENTED_EDGE('',*,*,#1720,.F.);
#2305=ORIENTED_EDGE('',*,*,#1721,.T.);
#2306=ORIENTED_EDGE('',*,*,#1720,.T.);
#2307=ORIENTED_EDGE('',*,*,#1722,.F.);
#2308=ORIENTED_EDGE('',*,*,#1723,.F.);
#2309=ORIENTED_EDGE('',*,*,#1724,.T.);
#2310=ORIENTED_EDGE('',*,*,#1723,.T.);
#2311=ORIENTED_EDGE('',*,*,#1725,.F.);
#2312=ORIENTED_EDGE('',*,*,#1726,.F.);
#2313=ORIENTED_EDGE('',*,*,#1727,.T.);
#2314=ORIENTED_EDGE('',*,*,#1726,.T.);
#2315=ORIENTED_EDGE('',*,*,#1728,.F.);
#2316=ORIENTED_EDGE('',*,*,#1729,.F.);
#2317=ORIENTED_EDGE('',*,*,#1730,.T.);
#2318=ORIENTED_EDGE('',*,*,#1729,.T.);
#2319=ORIENTED_EDGE('',*,*,#1731,.F.);
#2320=ORIENTED_EDGE('',*,*,#1732,.F.);
#2321=ORIENTED_EDGE('',*,*,#1733,.T.);
#2322=ORIENTED_EDGE('',*,*,#1732,.T.);
#2323=ORIENTED_EDGE('',*,*,#1734,.F.);
#2324=ORIENTED_EDGE('',*,*,#1735,.F.);
#2325=ORIENTED_EDGE('',*,*,#1736,.T.);
#2326=ORIENTED_EDGE('',*,*,#1735,.T.);
#2327=ORIENTED_EDGE('',*,*,#1737,.F.);
#2328=ORIENTED_EDGE('',*,*,#1738,.F.);
#2329=ORIENTED_EDGE('',*,*,#1739,.T.);
#2330=ORIENTED_EDGE('',*,*,#1738,.T.);
#2331=ORIENTED_EDGE('',*,*,#1740,.F.);
#2332=ORIENTED_EDGE('',*,*,#1741,.F.);
#2333=ORIENTED_EDGE('',*,*,#1742,.T.);
#2334=ORIENTED_EDGE('',*,*,#1741,.T.);
#2335=ORIENTED_EDGE('',*,*,#1743,.F.);
#2336=ORIENTED_EDGE('',*,*,#1744,.F.);
#2337=ORIENTED_EDGE('',*,*,#1745,.T.);
#2338=ORIENTED_EDGE('',*,*,#1744,.T.);
#2339=ORIENTED_EDGE('',*,*,#1746,.F.);
#2340=ORIENTED_EDGE('',*,*,#1747,.F.);
#2341=ORIENTED_EDGE('',*,*,#1748,.T.);
#2342=ORIENTED_EDGE('',*,*,#1747,.T.);
#2343=ORIENTED_EDGE('',*,*,#1749,.F.);
#2344=ORIENTED_EDGE('',*,*,#1750,.F.);
#2345=ORIENTED_EDGE('',*,*,#1751,.T.);
#2346=ORIENTED_EDGE('',*,*,#1750,.T.);
#2347=ORIENTED_EDGE('',*,*,#1752,.F.);
#2348=ORIENTED_EDGE('',*,*,#1753,.F.);
#2349=ORIENTED_EDGE('',*,*,#1754,.T.);
#2350=ORIENTED_EDGE('',*,*,#1753,.T.);
#2351=ORIENTED_EDGE('',*,*,#1755,.F.);
#2352=ORIENTED_EDGE('',*,*,#1756,.F.);
#2353=ORIENTED_EDGE('',*,*,#1757,.T.);
#2354=ORIENTED_EDGE('',*,*,#1756,.T.);
#2355=ORIENTED_EDGE('',*,*,#1758,.F.);
#2356=ORIENTED_EDGE('',*,*,#1715,.F.);
#2357=ORIENTED_EDGE('',*,*,#1758,.T.);
#2358=ORIENTED_EDGE('',*,*,#1755,.T.);
#2359=ORIENTED_EDGE('',*,*,#1752,.T.);
#2360=ORIENTED_EDGE('',*,*,#1749,.T.);
#2361=ORIENTED_EDGE('',*,*,#1746,.T.);
#2362=ORIENTED_EDGE('',*,*,#1743,.T.);
#2363=ORIENTED_EDGE('',*,*,#1740,.T.);
#2364=ORIENTED_EDGE('',*,*,#1737,.T.);
#2365=ORIENTED_EDGE('',*,*,#1734,.T.);
#2366=ORIENTED_EDGE('',*,*,#1731,.T.);
#2367=ORIENTED_EDGE('',*,*,#1728,.T.);
#2368=ORIENTED_EDGE('',*,*,#1725,.T.);
#2369=ORIENTED_EDGE('',*,*,#1722,.T.);
#2370=ORIENTED_EDGE('',*,*,#1719,.T.);
#2371=ORIENTED_EDGE('',*,*,#1716,.T.);
#2372=ORIENTED_EDGE('',*,*,#1711,.T.);
#2373=ORIENTED_EDGE('',*,*,#1757,.F.);
#2374=ORIENTED_EDGE('',*,*,#1714,.F.);
#2375=ORIENTED_EDGE('',*,*,#1718,.F.);
#2376=ORIENTED_EDGE('',*,*,#1721,.F.);
#2377=ORIENTED_EDGE('',*,*,#1724,.F.);
#2378=ORIENTED_EDGE('',*,*,#1727,.F.);
#2379=ORIENTED_EDGE('',*,*,#1730,.F.);
#2380=ORIENTED_EDGE('',*,*,#1733,.F.);
#2381=ORIENTED_EDGE('',*,*,#1736,.F.);
#2382=ORIENTED_EDGE('',*,*,#1739,.F.);
#2383=ORIENTED_EDGE('',*,*,#1742,.F.);
#2384=ORIENTED_EDGE('',*,*,#1745,.F.);
#2385=ORIENTED_EDGE('',*,*,#1748,.F.);
#2386=ORIENTED_EDGE('',*,*,#1751,.F.);
#2387=ORIENTED_EDGE('',*,*,#1754,.F.);
#2388=ORIENTED_EDGE('',*,*,#1713,.T.);
#2389=ORIENTED_EDGE('',*,*,#1759,.F.);
#2390=ORIENTED_EDGE('',*,*,#1760,.T.);
#2391=ORIENTED_EDGE('',*,*,#1761,.T.);
#2392=ORIENTED_EDGE('',*,*,#1760,.F.);
#2393=ORIENTED_EDGE('',*,*,#1762,.F.);
#2394=ORIENTED_EDGE('',*,*,#1763,.T.);
#2395=ORIENTED_EDGE('',*,*,#1764,.T.);
#2396=ORIENTED_EDGE('',*,*,#1763,.F.);
#2397=ORIENTED_EDGE('',*,*,#1762,.T.);
#2398=ORIENTED_EDGE('',*,*,#1759,.T.);
#2399=ORIENTED_EDGE('',*,*,#1764,.F.);
#2400=ORIENTED_EDGE('',*,*,#1761,.F.);
#2401=ORIENTED_EDGE('',*,*,#1765,.F.);
#2402=ORIENTED_EDGE('',*,*,#1766,.T.);
#2403=ORIENTED_EDGE('',*,*,#1767,.T.);
#2404=ORIENTED_EDGE('',*,*,#1766,.F.);
#2405=ORIENTED_EDGE('',*,*,#1768,.F.);
#2406=ORIENTED_EDGE('',*,*,#1769,.T.);
#2407=ORIENTED_EDGE('',*,*,#1770,.T.);
#2408=ORIENTED_EDGE('',*,*,#1769,.F.);
#2409=ORIENTED_EDGE('',*,*,#1768,.T.);
#2410=ORIENTED_EDGE('',*,*,#1765,.T.);
#2411=ORIENTED_EDGE('',*,*,#1770,.F.);
#2412=ORIENTED_EDGE('',*,*,#1767,.F.);
#2413=ORIENTED_EDGE('',*,*,#1771,.F.);
#2414=ORIENTED_EDGE('',*,*,#1772,.T.);
#2415=ORIENTED_EDGE('',*,*,#1773,.T.);
#2416=ORIENTED_EDGE('',*,*,#1772,.F.);
#2417=ORIENTED_EDGE('',*,*,#1774,.F.);
#2418=ORIENTED_EDGE('',*,*,#1775,.T.);
#2419=ORIENTED_EDGE('',*,*,#1776,.T.);
#2420=ORIENTED_EDGE('',*,*,#1775,.F.);
#2421=ORIENTED_EDGE('',*,*,#1774,.T.);
#2422=ORIENTED_EDGE('',*,*,#1771,.T.);
#2423=ORIENTED_EDGE('',*,*,#1776,.F.);
#2424=ORIENTED_EDGE('',*,*,#1773,.F.);
#2425=ORIENTED_EDGE('',*,*,#1777,.F.);
#2426=ORIENTED_EDGE('',*,*,#1778,.T.);
#2427=ORIENTED_EDGE('',*,*,#1779,.T.);
#2428=ORIENTED_EDGE('',*,*,#1778,.F.);
#2429=ORIENTED_EDGE('',*,*,#1780,.F.);
#2430=ORIENTED_EDGE('',*,*,#1781,.T.);
#2431=ORIENTED_EDGE('',*,*,#1782,.T.);
#2432=ORIENTED_EDGE('',*,*,#1781,.F.);
#2433=ORIENTED_EDGE('',*,*,#1780,.T.);
#2434=ORIENTED_EDGE('',*,*,#1777,.T.);
#2435=ORIENTED_EDGE('',*,*,#1782,.F.);
#2436=ORIENTED_EDGE('',*,*,#1779,.F.);
#2437=ORIENTED_EDGE('',*,*,#1783,.F.);
#2438=ORIENTED_EDGE('',*,*,#1784,.T.);
#2439=ORIENTED_EDGE('',*,*,#1785,.T.);
#2440=ORIENTED_EDGE('',*,*,#1784,.F.);
#2441=ORIENTED_EDGE('',*,*,#1786,.F.);
#2442=ORIENTED_EDGE('',*,*,#1787,.T.);
#2443=ORIENTED_EDGE('',*,*,#1788,.T.);
#2444=ORIENTED_EDGE('',*,*,#1787,.F.);
#2445=ORIENTED_EDGE('',*,*,#1786,.T.);
#2446=ORIENTED_EDGE('',*,*,#1783,.T.);
#2447=ORIENTED_EDGE('',*,*,#1788,.F.);
#2448=ORIENTED_EDGE('',*,*,#1785,.F.);
#2449=ORIENTED_EDGE('',*,*,#1789,.F.);
#2450=ORIENTED_EDGE('',*,*,#1790,.F.);
#2451=ORIENTED_EDGE('',*,*,#1791,.F.);
#2452=ORIENTED_EDGE('',*,*,#1792,.F.);
#2453=ORIENTED_EDGE('',*,*,#1793,.F.);
#2454=ORIENTED_EDGE('',*,*,#1794,.F.);
#2455=ORIENTED_EDGE('',*,*,#1795,.F.);
#2456=ORIENTED_EDGE('',*,*,#1796,.F.);
#2457=ORIENTED_EDGE('',*,*,#1796,.T.);
#2458=ORIENTED_EDGE('',*,*,#1797,.F.);
#2459=ORIENTED_EDGE('',*,*,#1790,.T.);
#2460=ORIENTED_EDGE('',*,*,#1798,.F.);
#2461=ORIENTED_EDGE('',*,*,#1793,.T.);
#2462=ORIENTED_EDGE('',*,*,#1798,.T.);
#2463=ORIENTED_EDGE('',*,*,#1789,.T.);
#2464=ORIENTED_EDGE('',*,*,#1799,.F.);
#2465=ORIENTED_EDGE('',*,*,#1795,.T.);
#2466=ORIENTED_EDGE('',*,*,#1800,.F.);
#2467=ORIENTED_EDGE('',*,*,#1791,.T.);
#2468=ORIENTED_EDGE('',*,*,#1797,.T.);
#2469=ORIENTED_EDGE('',*,*,#1794,.T.);
#2470=ORIENTED_EDGE('',*,*,#1799,.T.);
#2471=ORIENTED_EDGE('',*,*,#1792,.T.);
#2472=ORIENTED_EDGE('',*,*,#1800,.T.);
#2473=CYLINDRICAL_SURFACE('',#2830,4.);
#2474=CYLINDRICAL_SURFACE('',#2833,5.);
#2475=CYLINDRICAL_SURFACE('',#2836,4.5);
#2476=CYLINDRICAL_SURFACE('',#2839,4.5);
#2477=CYLINDRICAL_SURFACE('',#2842,4.5);
#2478=CYLINDRICAL_SURFACE('',#2845,4.5);
#2479=CYLINDRICAL_SURFACE('',#2859,6.);
#2480=CYLINDRICAL_SURFACE('',#2905,7.);
#2481=CYLINDRICAL_SURFACE('',#2908,4.);
#2482=CYLINDRICAL_SURFACE('',#2911,6.);
#2483=CYLINDRICAL_SURFACE('',#2925,4.);
#2484=CYLINDRICAL_SURFACE('',#2932,5.);
#2485=CYLINDRICAL_SURFACE('',#2937,8.);
#2486=CYLINDRICAL_SURFACE('',#2940,5.);
#2487=CYLINDRICAL_SURFACE('',#2943,3.);
#2488=CYLINDRICAL_SURFACE('',#2950,4.);
#2489=CYLINDRICAL_SURFACE('',#2955,6.);
#2490=CYLINDRICAL_SURFACE('',#2958,4.);
#2491=CYLINDRICAL_SURFACE('',#2961,3.);
#2492=CYLINDRICAL_SURFACE('',#2968,4.);
#2493=CYLINDRICAL_SURFACE('',#2973,6.);
#2494=CYLINDRICAL_SURFACE('',#2976,4.);
#2495=CYLINDRICAL_SURFACE('',#2984,4.);
#2496=CYLINDRICAL_SURFACE('',#2986,8.);
#2497=CYLINDRICAL_SURFACE('',#2990,5.);
#2498=CYLINDRICAL_SURFACE('',#3011,5.);
#2499=CYLINDRICAL_SURFACE('',#3014,6.);
#2500=CYLINDRICAL_SURFACE('',#3020,4.);
#2501=CYLINDRICAL_SURFACE('',#3023,5.);
#2502=CYLINDRICAL_SURFACE('',#3029,5.);
#2503=CYLINDRICAL_SURFACE('',#3032,10.);
#2504=CYLINDRICAL_SURFACE('',#3038,4.);
#2505=CYLINDRICAL_SURFACE('',#3041,7.);
#2506=CYLINDRICAL_SURFACE('',#3047,4.);
#2507=CYLINDRICAL_SURFACE('',#3050,8.);
#2508=CYLINDRICAL_SURFACE('',#3061,3.);
#2509=CYLINDRICAL_SURFACE('',#3063,6.);
#2510=ADVANCED_FACE('',(#304),#2473,.F.);
#2511=ADVANCED_FACE('',(#305),#2474,.F.);
#2512=ADVANCED_FACE('',(#306),#2475,.F.);
#2513=ADVANCED_FACE('',(#307),#2476,.F.);
#2514=ADVANCED_FACE('',(#308),#2477,.F.);
#2515=ADVANCED_FACE('',(#309),#2478,.F.);
#2516=ADVANCED_FACE('',(#310,#151,#152),#192,.T.);
#2517=ADVANCED_FACE('',(#311,#153,#154),#193,.T.);
#2518=ADVANCED_FACE('',(#312,#155,#156,#157,#158),#194,.T.);
#2519=ADVANCED_FACE('',(#313),#195,.T.);
#2520=ADVANCED_FACE('',(#314),#196,.F.);
#2521=ADVANCED_FACE('',(#315),#197,.T.);
#2522=ADVANCED_FACE('',(#316),#198,.T.);
#2523=ADVANCED_FACE('',(#317),#199,.T.);
#2524=ADVANCED_FACE('',(#318,#159,#160),#200,.T.);
#2525=ADVANCED_FACE('',(#319,#161,#162),#201,.F.);
#2526=ADVANCED_FACE('',(#320),#2479,.F.);
#2527=ADVANCED_FACE('',(#321),#202,.T.);
#2528=ADVANCED_FACE('',(#322),#203,.T.);
#2529=ADVANCED_FACE('',(#323),#204,.T.);
#2530=ADVANCED_FACE('',(#324),#205,.T.);
#2531=ADVANCED_FACE('',(#325),#206,.T.);
#2532=ADVANCED_FACE('',(#326),#207,.T.);
#2533=ADVANCED_FACE('',(#327),#208,.T.);
#2534=ADVANCED_FACE('',(#328),#209,.T.);
#2535=ADVANCED_FACE('',(#329),#210,.T.);
#2536=ADVANCED_FACE('',(#330),#211,.T.);
#2537=ADVANCED_FACE('',(#331),#212,.T.);
#2538=ADVANCED_FACE('',(#332),#213,.T.);
#2539=ADVANCED_FACE('',(#333),#214,.T.);
#2540=ADVANCED_FACE('',(#334),#215,.T.);
#2541=ADVANCED_FACE('',(#335),#216,.T.);
#2542=ADVANCED_FACE('',(#336),#217,.T.);
#2543=ADVANCED_FACE('',(#337),#218,.T.);
#2544=ADVANCED_FACE('',(#338),#219,.T.);
#2545=ADVANCED_FACE('',(#339),#220,.T.);
#2546=ADVANCED_FACE('',(#340),#221,.T.);
#2547=ADVANCED_FACE('',(#341),#222,.T.);
#2548=ADVANCED_FACE('',(#342),#223,.T.);
#2549=ADVANCED_FACE('',(#343),#224,.T.);
#2550=ADVANCED_FACE('',(#344),#225,.T.);
#2551=ADVANCED_FACE('',(#345),#226,.T.);
#2552=ADVANCED_FACE('',(#346),#227,.T.);
#2553=ADVANCED_FACE('',(#347),#228,.T.);
#2554=ADVANCED_FACE('',(#348),#229,.T.);
#2555=ADVANCED_FACE('',(#349),#230,.T.);
#2556=ADVANCED_FACE('',(#350),#231,.T.);
#2557=ADVANCED_FACE('',(#351),#232,.T.);
#2558=ADVANCED_FACE('',(#352),#233,.T.);
#2559=ADVANCED_FACE('',(#353),#234,.T.);
#2560=ADVANCED_FACE('',(#354),#235,.T.);
#2561=ADVANCED_FACE('',(#355),#236,.T.);
#2562=ADVANCED_FACE('',(#356),#237,.T.);
#2563=ADVANCED_FACE('',(#357),#238,.T.);
#2564=ADVANCED_FACE('',(#358),#239,.T.);
#2565=ADVANCED_FACE('',(#359),#240,.T.);
#2566=ADVANCED_FACE('',(#360),#241,.T.);
#2567=ADVANCED_FACE('',(#361,#163),#242,.T.);
#2568=ADVANCED_FACE('',(#362,#164),#243,.F.);
#2569=ADVANCED_FACE('',(#363),#2480,.F.);
#2570=ADVANCED_FACE('',(#364),#2481,.F.);
#2571=ADVANCED_FACE('',(#365),#2482,.F.);
#2572=ADVANCED_FACE('',(#366),#244,.T.);
#2573=ADVANCED_FACE('',(#367),#245,.T.);
#2574=ADVANCED_FACE('',(#368),#246,.T.);
#2575=ADVANCED_FACE('',(#369),#247,.T.);
#2576=ADVANCED_FACE('',(#370),#248,.T.);
#2577=ADVANCED_FACE('',(#371),#249,.T.);
#2578=ADVANCED_FACE('',(#372),#250,.T.);
#2579=ADVANCED_FACE('',(#373),#251,.T.);
#2580=ADVANCED_FACE('',(#374,#165,#166,#167),#252,.T.);
#2581=ADVANCED_FACE('',(#375,#168,#169,#170),#253,.F.);
#2582=ADVANCED_FACE('',(#376),#2483,.T.);
#2583=ADVANCED_FACE('',(#377,#171),#254,.F.);
#2584=ADVANCED_FACE('',(#378,#172),#255,.F.);
#2585=ADVANCED_FACE('',(#379),#2484,.T.);
#2586=ADVANCED_FACE('',(#380,#173),#256,.T.);
#2587=ADVANCED_FACE('',(#381),#2485,.T.);
#2588=ADVANCED_FACE('',(#382),#257,.F.);
#2589=ADVANCED_FACE('',(#383),#2486,.T.);
#2590=ADVANCED_FACE('',(#384),#258,.T.);
#2591=ADVANCED_FACE('',(#385),#2487,.T.);
#2592=ADVANCED_FACE('',(#386,#174),#259,.F.);
#2593=ADVANCED_FACE('',(#387,#175),#260,.F.);
#2594=ADVANCED_FACE('',(#388),#2488,.T.);
#2595=ADVANCED_FACE('',(#389,#176),#261,.T.);
#2596=ADVANCED_FACE('',(#390),#2489,.T.);
#2597=ADVANCED_FACE('',(#391),#262,.F.);
#2598=ADVANCED_FACE('',(#392),#2490,.T.);
#2599=ADVANCED_FACE('',(#393),#263,.T.);
#2600=ADVANCED_FACE('',(#394),#2491,.T.);
#2601=ADVANCED_FACE('',(#395,#177),#264,.F.);
#2602=ADVANCED_FACE('',(#396,#178),#265,.F.);
#2603=ADVANCED_FACE('',(#397),#2492,.T.);
#2604=ADVANCED_FACE('',(#398,#179),#266,.T.);
#2605=ADVANCED_FACE('',(#399),#2493,.T.);
#2606=ADVANCED_FACE('',(#400),#267,.F.);
#2607=ADVANCED_FACE('',(#401),#2494,.T.);
#2608=ADVANCED_FACE('',(#402),#268,.T.);
#2609=ADVANCED_FACE('',(#403),#269,.F.);
#2610=ADVANCED_FACE('',(#404),#270,.F.);
#2611=ADVANCED_FACE('',(#405),#271,.F.);
#2612=ADVANCED_FACE('',(#406),#2495,.F.);
#2613=ADVANCED_FACE('',(#407),#2496,.T.);
#2614=ADVANCED_FACE('',(#408),#272,.T.);
#2615=ADVANCED_FACE('',(#409),#2497,.F.);
#2616=ADVANCED_FACE('',(#410),#273,.T.);
#2617=ADVANCED_FACE('',(#411),#274,.T.);
#2618=ADVANCED_FACE('',(#412),#275,.T.);
#2619=ADVANCED_FACE('',(#413),#276,.T.);
#2620=ADVANCED_FACE('',(#414),#277,.T.);
#2621=ADVANCED_FACE('',(#415),#278,.T.);
#2622=ADVANCED_FACE('',(#416),#279,.T.);
#2623=ADVANCED_FACE('',(#417),#280,.T.);
#2624=ADVANCED_FACE('',(#418),#281,.T.);
#2625=ADVANCED_FACE('',(#419),#282,.T.);
#2626=ADVANCED_FACE('',(#420),#283,.T.);
#2627=ADVANCED_FACE('',(#421),#284,.T.);
#2628=ADVANCED_FACE('',(#422),#285,.T.);
#2629=ADVANCED_FACE('',(#423),#286,.T.);
#2630=ADVANCED_FACE('',(#424),#287,.T.);
#2631=ADVANCED_FACE('',(#425,#180),#288,.T.);
#2632=ADVANCED_FACE('',(#426,#181),#289,.F.);
#2633=ADVANCED_FACE('',(#427),#2498,.F.);
#2634=ADVANCED_FACE('',(#428),#2499,.T.);
#2635=ADVANCED_FACE('',(#429,#182),#290,.T.);
#2636=ADVANCED_FACE('',(#430,#183),#291,.F.);
#2637=ADVANCED_FACE('',(#431),#2500,.F.);
#2638=ADVANCED_FACE('',(#432),#2501,.T.);
#2639=ADVANCED_FACE('',(#433,#184),#292,.T.);
#2640=ADVANCED_FACE('',(#434,#185),#293,.F.);
#2641=ADVANCED_FACE('',(#435),#2502,.F.);
#2642=ADVANCED_FACE('',(#436),#2503,.T.);
#2643=ADVANCED_FACE('',(#437,#186),#294,.T.);
#2644=ADVANCED_FACE('',(#438,#187),#295,.F.);
#2645=ADVANCED_FACE('',(#439),#2504,.F.);
#2646=ADVANCED_FACE('',(#440),#2505,.T.);
#2647=ADVANCED_FACE('',(#441,#188),#296,.T.);
#2648=ADVANCED_FACE('',(#442,#189),#297,.F.);
#2649=ADVANCED_FACE('',(#443),#2506,.F.);
#2650=ADVANCED_FACE('',(#444),#2507,.T.);
#2651=ADVANCED_FACE('',(#445,#190),#298,.T.);
#2652=ADVANCED_FACE('',(#446,#191),#299,.F.);
#2653=ADVANCED_FACE('',(#447),#300,.F.);
#2654=ADVANCED_FACE('',(#448),#301,.F.);
#2655=ADVANCED_FACE('',(#449),#302,.F.);
#2656=ADVANCED_FACE('',(#450),#2508,.F.);
#2657=ADVANCED_FACE('',(#451),#2509,.T.);
#2658=ADVANCED_FACE('',(#452),#303,.T.);
#2659=CLOSED_SHELL('',(#2510,#2511,#2512,#2513,#2514,#2515,#2516,#2517,
#2518,#2519,#2520,#2521,#2522,#2523,#2524,#2525));
#2660=CLOSED_SHELL('',(#2526,#2527,#2528,#2529,#2530,#2531,#2532,#2533,
#2534,#2535,#2536,#2537,#2538,#2539,#2540,#2541,#2542,#2543,#2544,#2545,
#2546,#2547,#2548,#2549,#2550,#2551,#2552,#2553,#2554,#2555,#2556,#2557,
#2558,#2559,#2560,#2561,#2562,#2563,#2564,#2565,#2566,#2567,#2568));
#2661=CLOSED_SHELL('',(#2569,#2570,#2571,#2572,#2573,#2574,#2575,#2576,
#2577,#2578,#2579,#2580,#2581));
#2662=CLOSED_SHELL('',(#2582,#2583,#2584,#2585,#2586,#2587,#2588,#2589,
#2590));
#2663=CLOSED_SHELL('',(#2591,#2592,#2593,#2594,#2595,#2596,#2597,#2598,
#2599));
#2664=CLOSED_SHELL('',(#2600,#2601,#2602,#2603,#2604,#2605,#2606,#2607,
#2608));
#2665=CLOSED_SHELL('',(#2609,#2610,#2611,#2612,#2613,#2614));
#2666=CLOSED_SHELL('',(#2615,#2616,#2617,#2618,#2619,#2620,#2621,#2622,
#2623,#2624,#2625,#2626,#2627,#2628,#2629,#2630,#2631,#2632));
#2667=CLOSED_SHELL('',(#2633,#2634,#2635,#2636));
#2668=CLOSED_SHELL('',(#2637,#2638,#2639,#2640));
#2669=CLOSED_SHELL('',(#2641,#2642,#2643,#2644));
#2670=CLOSED_SHELL('',(#2645,#2646,#2647,#2648));
#2671=CLOSED_SHELL('',(#2649,#2650,#2651,#2652));
#2672=CLOSED_SHELL('',(#2653,#2654,#2655,#2656,#2657,#2658));
#2673=DERIVED_UNIT_ELEMENT(#2701,1.);
#2674=DERIVED_UNIT_ELEMENT(#4645,-3.);
#2675=DERIVED_UNIT_ELEMENT(#2701,1.);
#2676=DERIVED_UNIT_ELEMENT(#4645,-3.);
#2677=DERIVED_UNIT_ELEMENT(#2701,1.);
#2678=DERIVED_UNIT_ELEMENT(#4645,-3.);
#2679=DERIVED_UNIT_ELEMENT(#2701,1.);
#2680=DERIVED_UNIT_ELEMENT(#4645,-3.);
#2681=DERIVED_UNIT_ELEMENT(#2701,1.);
#2682=DERIVED_UNIT_ELEMENT(#4645,-3.);
#2683=DERIVED_UNIT_ELEMENT(#2701,1.);
#2684=DERIVED_UNIT_ELEMENT(#4645,-3.);
#2685=DERIVED_UNIT_ELEMENT(#2701,1.);
#2686=DERIVED_UNIT_ELEMENT(#4645,-3.);
#2687=DERIVED_UNIT_ELEMENT(#2701,1.);
#2688=DERIVED_UNIT_ELEMENT(#4645,-3.);
#2689=DERIVED_UNIT_ELEMENT(#2701,1.);
#2690=DERIVED_UNIT_ELEMENT(#4645,-3.);
#2691=DERIVED_UNIT_ELEMENT(#2701,1.);
#2692=DERIVED_UNIT_ELEMENT(#4645,-3.);
#2693=DERIVED_UNIT_ELEMENT(#2701,1.);
#2694=DERIVED_UNIT_ELEMENT(#4645,-3.);
#2695=DERIVED_UNIT_ELEMENT(#2701,1.);
#2696=DERIVED_UNIT_ELEMENT(#4645,-3.);
#2697=DERIVED_UNIT_ELEMENT(#2701,1.);
#2698=DERIVED_UNIT_ELEMENT(#4645,-3.);
#2699=DERIVED_UNIT_ELEMENT(#2701,1.);
#2700=DERIVED_UNIT_ELEMENT(#4645,-3.);
#2701=(
MASS_UNIT()
NAMED_UNIT(*)
SI_UNIT(.KILO.,.GRAM.)
);
#2702=DERIVED_UNIT((#2673,#2674));
#2703=DERIVED_UNIT((#2675,#2676));
#2704=DERIVED_UNIT((#2677,#2678));
#2705=DERIVED_UNIT((#2679,#2680));
#2706=DERIVED_UNIT((#2681,#2682));
#2707=DERIVED_UNIT((#2683,#2684));
#2708=DERIVED_UNIT((#2685,#2686));
#2709=DERIVED_UNIT((#2687,#2688));
#2710=DERIVED_UNIT((#2689,#2690));
#2711=DERIVED_UNIT((#2691,#2692));
#2712=DERIVED_UNIT((#2693,#2694));
#2713=DERIVED_UNIT((#2695,#2696));
#2714=DERIVED_UNIT((#2697,#2698));
#2715=DERIVED_UNIT((#2699,#2700));
#2716=MEASURE_REPRESENTATION_ITEM('density measure',
POSITIVE_RATIO_MEASURE(7850.),#2702);
#2717=MEASURE_REPRESENTATION_ITEM('density measure',
POSITIVE_RATIO_MEASURE(7850.),#2703);
#2718=MEASURE_REPRESENTATION_ITEM('density measure',
POSITIVE_RATIO_MEASURE(7850.),#2704);
#2719=MEASURE_REPRESENTATION_ITEM('density measure',
POSITIVE_RATIO_MEASURE(7850.),#2705);
#2720=MEASURE_REPRESENTATION_ITEM('density measure',
POSITIVE_RATIO_MEASURE(7850.),#2706);
#2721=MEASURE_REPRESENTATION_ITEM('density measure',
POSITIVE_RATIO_MEASURE(7850.),#2707);
#2722=MEASURE_REPRESENTATION_ITEM('density measure',
POSITIVE_RATIO_MEASURE(7850.),#2708);
#2723=MEASURE_REPRESENTATION_ITEM('density measure',
POSITIVE_RATIO_MEASURE(7850.),#2709);
#2724=MEASURE_REPRESENTATION_ITEM('density measure',
POSITIVE_RATIO_MEASURE(8920.),#2710);
#2725=MEASURE_REPRESENTATION_ITEM('density measure',
POSITIVE_RATIO_MEASURE(8920.),#2711);
#2726=MEASURE_REPRESENTATION_ITEM('density measure',
POSITIVE_RATIO_MEASURE(7850.),#2712);
#2727=MEASURE_REPRESENTATION_ITEM('density measure',
POSITIVE_RATIO_MEASURE(7850.),#2713);
#2728=MEASURE_REPRESENTATION_ITEM('density measure',
POSITIVE_RATIO_MEASURE(7850.),#2714);
#2729=MEASURE_REPRESENTATION_ITEM('density measure',
POSITIVE_RATIO_MEASURE(7850.),#2715);
#2730=PROPERTY_DEFINITION_REPRESENTATION(#2800,#2758);
#2731=PROPERTY_DEFINITION_REPRESENTATION(#2801,#2759);
#2732=PROPERTY_DEFINITION_REPRESENTATION(#2802,#2760);
#2733=PROPERTY_DEFINITION_REPRESENTATION(#2803,#2761);
#2734=PROPERTY_DEFINITION_REPRESENTATION(#2804,#2762);
#2735=PROPERTY_DEFINITION_REPRESENTATION(#2805,#2763);
#2736=PROPERTY_DEFINITION_REPRESENTATION(#2806,#2764);
#2737=PROPERTY_DEFINITION_REPRESENTATION(#2807,#2765);
#2738=PROPERTY_DEFINITION_REPRESENTATION(#2808,#2766);
#2739=PROPERTY_DEFINITION_REPRESENTATION(#2809,#2767);
#2740=PROPERTY_DEFINITION_REPRESENTATION(#2810,#2768);
#2741=PROPERTY_DEFINITION_REPRESENTATION(#2811,#2769);
#2742=PROPERTY_DEFINITION_REPRESENTATION(#2812,#2770);
#2743=PROPERTY_DEFINITION_REPRESENTATION(#2813,#2771);
#2744=PROPERTY_DEFINITION_REPRESENTATION(#2814,#2772);
#2745=PROPERTY_DEFINITION_REPRESENTATION(#2815,#2773);
#2746=PROPERTY_DEFINITION_REPRESENTATION(#2816,#2774);
#2747=PROPERTY_DEFINITION_REPRESENTATION(#2817,#2775);
#2748=PROPERTY_DEFINITION_REPRESENTATION(#2818,#2776);
#2749=PROPERTY_DEFINITION_REPRESENTATION(#2819,#2777);
#2750=PROPERTY_DEFINITION_REPRESENTATION(#2820,#2778);
#2751=PROPERTY_DEFINITION_REPRESENTATION(#2821,#2779);
#2752=PROPERTY_DEFINITION_REPRESENTATION(#2822,#2780);
#2753=PROPERTY_DEFINITION_REPRESENTATION(#2823,#2781);
#2754=PROPERTY_DEFINITION_REPRESENTATION(#2824,#2782);
#2755=PROPERTY_DEFINITION_REPRESENTATION(#2825,#2783);
#2756=PROPERTY_DEFINITION_REPRESENTATION(#2826,#2784);
#2757=PROPERTY_DEFINITION_REPRESENTATION(#2827,#2785);
#2758=REPRESENTATION('material name',(#2786),#4629);
#2759=REPRESENTATION('density',(#2716),#4629);
#2760=REPRESENTATION('material name',(#2787),#4630);
#2761=REPRESENTATION('density',(#2717),#4630);
#2762=REPRESENTATION('material name',(#2788),#4631);
#2763=REPRESENTATION('density',(#2718),#4631);
#2764=REPRESENTATION('material name',(#2789),#4632);
#2765=REPRESENTATION('density',(#2719),#4632);
#2766=REPRESENTATION('material name',(#2790),#4633);
#2767=REPRESENTATION('density',(#2720),#4633);
#2768=REPRESENTATION('material name',(#2791),#4634);
#2769=REPRESENTATION('density',(#2721),#4634);
#2770=REPRESENTATION('material name',(#2792),#4635);
#2771=REPRESENTATION('density',(#2722),#4635);
#2772=REPRESENTATION('material name',(#2793),#4636);
#2773=REPRESENTATION('density',(#2723),#4636);
#2774=REPRESENTATION('material name',(#2794),#4637);
#2775=REPRESENTATION('density',(#2724),#4637);
#2776=REPRESENTATION('material name',(#2795),#4638);
#2777=REPRESENTATION('density',(#2725),#4638);
#2778=REPRESENTATION('material name',(#2796),#4639);
#2779=REPRESENTATION('density',(#2726),#4639);
#2780=REPRESENTATION('material name',(#2797),#4640);
#2781=REPRESENTATION('density',(#2727),#4640);
#2782=REPRESENTATION('material name',(#2798),#4641);
#2783=REPRESENTATION('density',(#2728),#4641);
#2784=REPRESENTATION('material name',(#2799),#4642);
#2785=REPRESENTATION('density',(#2729),#4642);
#2786=DESCRIPTIVE_REPRESENTATION_ITEM('Steel','Steel');
#2787=DESCRIPTIVE_REPRESENTATION_ITEM('Steel','Steel');
#2788=DESCRIPTIVE_REPRESENTATION_ITEM('Steel','Steel');
#2789=DESCRIPTIVE_REPRESENTATION_ITEM('Steel','Steel');
#2790=DESCRIPTIVE_REPRESENTATION_ITEM('Steel','Steel');
#2791=DESCRIPTIVE_REPRESENTATION_ITEM('Steel','Steel');
#2792=DESCRIPTIVE_REPRESENTATION_ITEM('Steel','Steel');
#2793=DESCRIPTIVE_REPRESENTATION_ITEM('Steel','Steel');
#2794=DESCRIPTIVE_REPRESENTATION_ITEM('Copper, Alloy','Copper, Alloy');
#2795=DESCRIPTIVE_REPRESENTATION_ITEM('Copper, Alloy','Copper, Alloy');
#2796=DESCRIPTIVE_REPRESENTATION_ITEM('Steel','Steel');
#2797=DESCRIPTIVE_REPRESENTATION_ITEM('Steel','Steel');
#2798=DESCRIPTIVE_REPRESENTATION_ITEM('Steel','Steel');
#2799=DESCRIPTIVE_REPRESENTATION_ITEM('Steel','Steel');
#2800=PROPERTY_DEFINITION('material property','material name',#4716);
#2801=PROPERTY_DEFINITION('material property','density of part',#4716);
#2802=PROPERTY_DEFINITION('material property','material name',#4717);
#2803=PROPERTY_DEFINITION('material property','density of part',#4717);
#2804=PROPERTY_DEFINITION('material property','material name',#4718);
#2805=PROPERTY_DEFINITION('material property','density of part',#4718);
#2806=PROPERTY_DEFINITION('material property','material name',#4719);
#2807=PROPERTY_DEFINITION('material property','density of part',#4719);
#2808=PROPERTY_DEFINITION('material property','material name',#4720);
#2809=PROPERTY_DEFINITION('material property','density of part',#4720);
#2810=PROPERTY_DEFINITION('material property','material name',#4721);
#2811=PROPERTY_DEFINITION('material property','density of part',#4721);
#2812=PROPERTY_DEFINITION('material property','material name',#4722);
#2813=PROPERTY_DEFINITION('material property','density of part',#4722);
#2814=PROPERTY_DEFINITION('material property','material name',#4723);
#2815=PROPERTY_DEFINITION('material property','density of part',#4723);
#2816=PROPERTY_DEFINITION('material property','material name',#4724);
#2817=PROPERTY_DEFINITION('material property','density of part',#4724);
#2818=PROPERTY_DEFINITION('material property','material name',#4725);
#2819=PROPERTY_DEFINITION('material property','density of part',#4725);
#2820=PROPERTY_DEFINITION('material property','material name',#4726);
#2821=PROPERTY_DEFINITION('material property','density of part',#4726);
#2822=PROPERTY_DEFINITION('material property','material name',#4727);
#2823=PROPERTY_DEFINITION('material property','density of part',#4727);
#2824=PROPERTY_DEFINITION('material property','material name',#4728);
#2825=PROPERTY_DEFINITION('material property','density of part',#4728);
#2826=PROPERTY_DEFINITION('material property','material name',#4729);
#2827=PROPERTY_DEFINITION('material property','density of part',#4729);
#2828=AXIS2_PLACEMENT_3D('',#3867,#3087,#3088);
#2829=AXIS2_PLACEMENT_3D('',#3868,#3089,#3090);
#2830=AXIS2_PLACEMENT_3D('',#3869,#3091,#3092);
#2831=AXIS2_PLACEMENT_3D('',#3871,#3093,#3094);
#2832=AXIS2_PLACEMENT_3D('',#3874,#3096,#3097);
#2833=AXIS2_PLACEMENT_3D('',#3875,#3098,#3099);
#2834=AXIS2_PLACEMENT_3D('',#3877,#3100,#3101);
#2835=AXIS2_PLACEMENT_3D('',#3880,#3103,#3104);
#2836=AXIS2_PLACEMENT_3D('',#3881,#3105,#3106);
#2837=AXIS2_PLACEMENT_3D('',#3883,#3107,#3108);
#2838=AXIS2_PLACEMENT_3D('',#3886,#3110,#3111);
#2839=AXIS2_PLACEMENT_3D('',#3887,#3112,#3113);
#2840=AXIS2_PLACEMENT_3D('',#3889,#3114,#3115);
#2841=AXIS2_PLACEMENT_3D('',#3892,#3117,#3118);
#2842=AXIS2_PLACEMENT_3D('',#3893,#3119,#3120);
#2843=AXIS2_PLACEMENT_3D('',#3895,#3121,#3122);
#2844=AXIS2_PLACEMENT_3D('',#3898,#3124,#3125);
#2845=AXIS2_PLACEMENT_3D('',#3899,#3126,#3127);
#2846=AXIS2_PLACEMENT_3D('',#3901,#3128,#3129);
#2847=AXIS2_PLACEMENT_3D('',#3904,#3131,#3132);
#2848=AXIS2_PLACEMENT_3D('',#3905,#3133,#3134);
#2849=AXIS2_PLACEMENT_3D('',#3914,#3139,#3140);
#2850=AXIS2_PLACEMENT_3D('',#3923,#3145,#3146);
#2851=AXIS2_PLACEMENT_3D('',#3932,#3151,#3152);
#2852=AXIS2_PLACEMENT_3D('',#3935,#3155,#3156);
#2853=AXIS2_PLACEMENT_3D('',#3938,#3159,#3160);
#2854=AXIS2_PLACEMENT_3D('',#3947,#3165,#3166);
#2855=AXIS2_PLACEMENT_3D('',#3950,#3169,#3170);
#2856=AXIS2_PLACEMENT_3D('',#3953,#3173,#3174);
#2857=AXIS2_PLACEMENT_3D('',#3954,#3175,#3176);
#2858=AXIS2_PLACEMENT_3D('',#3955,#3177,#3178);
#2859=AXIS2_PLACEMENT_3D('',#3956,#3179,#3180);
#2860=AXIS2_PLACEMENT_3D('',#3958,#3181,#3182);
#2861=AXIS2_PLACEMENT_3D('',#3961,#3184,#3185);
#2862=AXIS2_PLACEMENT_3D('',#3962,#3186,#3187);
#2863=AXIS2_PLACEMENT_3D('',#3971,#3192,#3193);
#2864=AXIS2_PLACEMENT_3D('',#3977,#3197,#3198);
#2865=AXIS2_PLACEMENT_3D('',#3983,#3202,#3203);
#2866=AXIS2_PLACEMENT_3D('',#3989,#3207,#3208);
#2867=AXIS2_PLACEMENT_3D('',#3995,#3212,#3213);
#2868=AXIS2_PLACEMENT_3D('',#4001,#3217,#3218);
#2869=AXIS2_PLACEMENT_3D('',#4007,#3222,#3223);
#2870=AXIS2_PLACEMENT_3D('',#4013,#3227,#3228);
#2871=AXIS2_PLACEMENT_3D('',#4019,#3232,#3233);
#2872=AXIS2_PLACEMENT_3D('',#4025,#3237,#3238);
#2873=AXIS2_PLACEMENT_3D('',#4031,#3242,#3243);
#2874=AXIS2_PLACEMENT_3D('',#4037,#3247,#3248);
#2875=AXIS2_PLACEMENT_3D('',#4043,#3252,#3253);
#2876=AXIS2_PLACEMENT_3D('',#4049,#3257,#3258);
#2877=AXIS2_PLACEMENT_3D('',#4055,#3262,#3263);
#2878=AXIS2_PLACEMENT_3D('',#4061,#3267,#3268);
#2879=AXIS2_PLACEMENT_3D('',#4067,#3272,#3273);
#2880=AXIS2_PLACEMENT_3D('',#4073,#3277,#3278);
#2881=AXIS2_PLACEMENT_3D('',#4079,#3282,#3283);
#2882=AXIS2_PLACEMENT_3D('',#4085,#3287,#3288);
#2883=AXIS2_PLACEMENT_3D('',#4091,#3292,#3293);
#2884=AXIS2_PLACEMENT_3D('',#4097,#3297,#3298);
#2885=AXIS2_PLACEMENT_3D('',#4103,#3302,#3303);
#2886=AXIS2_PLACEMENT_3D('',#4109,#3307,#3308);
#2887=AXIS2_PLACEMENT_3D('',#4115,#3312,#3313);
#2888=AXIS2_PLACEMENT_3D('',#4121,#3317,#3318);
#2889=AXIS2_PLACEMENT_3D('',#4127,#3322,#3323);
#2890=AXIS2_PLACEMENT_3D('',#4133,#3327,#3328);
#2891=AXIS2_PLACEMENT_3D('',#4139,#3332,#3333);
#2892=AXIS2_PLACEMENT_3D('',#4145,#3337,#3338);
#2893=AXIS2_PLACEMENT_3D('',#4151,#3342,#3343);
#2894=AXIS2_PLACEMENT_3D('',#4157,#3347,#3348);
#2895=AXIS2_PLACEMENT_3D('',#4163,#3352,#3353);
#2896=AXIS2_PLACEMENT_3D('',#4169,#3357,#3358);
#2897=AXIS2_PLACEMENT_3D('',#4175,#3362,#3363);
#2898=AXIS2_PLACEMENT_3D('',#4181,#3367,#3368);
#2899=AXIS2_PLACEMENT_3D('',#4187,#3372,#3373);
#2900=AXIS2_PLACEMENT_3D('',#4193,#3377,#3378);
#2901=AXIS2_PLACEMENT_3D('',#4199,#3382,#3383);
#2902=AXIS2_PLACEMENT_3D('',#4202,#3386,#3387);
#2903=AXIS2_PLACEMENT_3D('',#4203,#3388,#3389);
#2904=AXIS2_PLACEMENT_3D('',#4204,#3390,#3391);
#2905=AXIS2_PLACEMENT_3D('',#4205,#3392,#3393);
#2906=AXIS2_PLACEMENT_3D('',#4207,#3394,#3395);
#2907=AXIS2_PLACEMENT_3D('',#4210,#3397,#3398);
#2908=AXIS2_PLACEMENT_3D('',#4211,#3399,#3400);
#2909=AXIS2_PLACEMENT_3D('',#4213,#3401,#3402);
#2910=AXIS2_PLACEMENT_3D('',#4216,#3404,#3405);
#2911=AXIS2_PLACEMENT_3D('',#4217,#3406,#3407);
#2912=AXIS2_PLACEMENT_3D('',#4219,#3408,#3409);
#2913=AXIS2_PLACEMENT_3D('',#4222,#3411,#3412);
#2914=AXIS2_PLACEMENT_3D('',#4223,#3413,#3414);
#2915=AXIS2_PLACEMENT_3D('',#4232,#3419,#3420);
#2916=AXIS2_PLACEMENT_3D('',#4238,#3424,#3425);
#2917=AXIS2_PLACEMENT_3D('',#4244,#3429,#3430);
#2918=AXIS2_PLACEMENT_3D('',#4250,#3434,#3435);
#2919=AXIS2_PLACEMENT_3D('',#4256,#3439,#3440);
#2920=AXIS2_PLACEMENT_3D('',#4262,#3444,#3445);
#2921=AXIS2_PLACEMENT_3D('',#4268,#3449,#3450);
#2922=AXIS2_PLACEMENT_3D('',#4271,#3453,#3454);
#2923=AXIS2_PLACEMENT_3D('',#4272,#3455,#3456);
#2924=AXIS2_PLACEMENT_3D('',#4273,#3457,#3458);
#2925=AXIS2_PLACEMENT_3D('',#4274,#3459,#3460);
#2926=AXIS2_PLACEMENT_3D('',#4276,#3461,#3462);
#2927=AXIS2_PLACEMENT_3D('',#4279,#3464,#3465);
#2928=AXIS2_PLACEMENT_3D('',#4280,#3466,#3467);
#2929=AXIS2_PLACEMENT_3D('',#4282,#3468,#3469);
#2930=AXIS2_PLACEMENT_3D('',#4283,#3470,#3471);
#2931=AXIS2_PLACEMENT_3D('',#4285,#3472,#3473);
#2932=AXIS2_PLACEMENT_3D('',#4286,#3474,#3475);
#2933=AXIS2_PLACEMENT_3D('',#4288,#3476,#3477);
#2934=AXIS2_PLACEMENT_3D('',#4290,#3479,#3480);
#2935=AXIS2_PLACEMENT_3D('',#4292,#3481,#3482);
#2936=AXIS2_PLACEMENT_3D('',#4294,#3483,#3484);
#2937=AXIS2_PLACEMENT_3D('',#4295,#3485,#3486);
#2938=AXIS2_PLACEMENT_3D('',#4298,#3488,#3489);
#2939=AXIS2_PLACEMENT_3D('',#4299,#3490,#3491);
#2940=AXIS2_PLACEMENT_3D('',#4300,#3492,#3493);
#2941=AXIS2_PLACEMENT_3D('',#4302,#3495,#3496);
#2942=AXIS2_PLACEMENT_3D('',#4303,#3497,#3498);
#2943=AXIS2_PLACEMENT_3D('',#4304,#3499,#3500);
#2944=AXIS2_PLACEMENT_3D('',#4306,#3501,#3502);
#2945=AXIS2_PLACEMENT_3D('',#4309,#3504,#3505);
#2946=AXIS2_PLACEMENT_3D('',#4310,#3506,#3507);
#2947=AXIS2_PLACEMENT_3D('',#4312,#3508,#3509);
#2948=AXIS2_PLACEMENT_3D('',#4313,#3510,#3511);
#2949=AXIS2_PLACEMENT_3D('',#4315,#3512,#3513);
#2950=AXIS2_PLACEMENT_3D('',#4316,#3514,#3515);
#2951=AXIS2_PLACEMENT_3D('',#4318,#3516,#3517);
#2952=AXIS2_PLACEMENT_3D('',#4320,#3519,#3520);
#2953=AXIS2_PLACEMENT_3D('',#4322,#3521,#3522);
#2954=AXIS2_PLACEMENT_3D('',#4324,#3523,#3524);
#2955=AXIS2_PLACEMENT_3D('',#4325,#3525,#3526);
#2956=AXIS2_PLACEMENT_3D('',#4328,#3528,#3529);
#2957=AXIS2_PLACEMENT_3D('',#4329,#3530,#3531);
#2958=AXIS2_PLACEMENT_3D('',#4330,#3532,#3533);
#2959=AXIS2_PLACEMENT_3D('',#4332,#3535,#3536);
#2960=AXIS2_PLACEMENT_3D('',#4333,#3537,#3538);
#2961=AXIS2_PLACEMENT_3D('',#4334,#3539,#3540);
#2962=AXIS2_PLACEMENT_3D('',#4336,#3541,#3542);
#2963=AXIS2_PLACEMENT_3D('',#4339,#3544,#3545);
#2964=AXIS2_PLACEMENT_3D('',#4340,#3546,#3547);
#2965=AXIS2_PLACEMENT_3D('',#4342,#3548,#3549);
#2966=AXIS2_PLACEMENT_3D('',#4343,#3550,#3551);
#2967=AXIS2_PLACEMENT_3D('',#4345,#3552,#3553);
#2968=AXIS2_PLACEMENT_3D('',#4346,#3554,#3555);
#2969=AXIS2_PLACEMENT_3D('',#4348,#3556,#3557);
#2970=AXIS2_PLACEMENT_3D('',#4350,#3559,#3560);
#2971=AXIS2_PLACEMENT_3D('',#4352,#3561,#3562);
#2972=AXIS2_PLACEMENT_3D('',#4354,#3563,#3564);
#2973=AXIS2_PLACEMENT_3D('',#4355,#3565,#3566);
#2974=AXIS2_PLACEMENT_3D('',#4358,#3568,#3569);
#2975=AXIS2_PLACEMENT_3D('',#4359,#3570,#3571);
#2976=AXIS2_PLACEMENT_3D('',#4360,#3572,#3573);
#2977=AXIS2_PLACEMENT_3D('',#4362,#3575,#3576);
#2978=AXIS2_PLACEMENT_3D('',#4363,#3577,#3578);
#2979=AXIS2_PLACEMENT_3D('',#4364,#3579,#3580);
#2980=AXIS2_PLACEMENT_3D('',#4373,#3585,#3586);
#2981=AXIS2_PLACEMENT_3D('',#4382,#3591,#3592);
#2982=AXIS2_PLACEMENT_3D('',#4383,#3593,#3594);
#2983=AXIS2_PLACEMENT_3D('',#4384,#3595,#3596);
#2984=AXIS2_PLACEMENT_3D('',#4385,#3597,#3598);
#2985=AXIS2_PLACEMENT_3D('',#4386,#3599,#3600);
#2986=AXIS2_PLACEMENT_3D('',#4387,#3601,#3602);
#2987=AXIS2_PLACEMENT_3D('',#4388,#3603,#3604);
#2988=AXIS2_PLACEMENT_3D('',#4389,#3605,#3606);
#2989=AXIS2_PLACEMENT_3D('',#4390,#3607,#3608);
#2990=AXIS2_PLACEMENT_3D('',#4391,#3609,#3610);
#2991=AXIS2_PLACEMENT_3D('',#4393,#3611,#3612);
#2992=AXIS2_PLACEMENT_3D('',#4396,#3614,#3615);
#2993=AXIS2_PLACEMENT_3D('',#4397,#3616,#3617);
#2994=AXIS2_PLACEMENT_3D('',#4406,#3622,#3623);
#2995=AXIS2_PLACEMENT_3D('',#4412,#3627,#3628);
#2996=AXIS2_PLACEMENT_3D('',#4418,#3632,#3633);
#2997=AXIS2_PLACEMENT_3D('',#4424,#3637,#3638);
#2998=AXIS2_PLACEMENT_3D('',#4430,#3642,#3643);
#2999=AXIS2_PLACEMENT_3D('',#4436,#3647,#3648);
#3000=AXIS2_PLACEMENT_3D('',#4442,#3652,#3653);
#3001=AXIS2_PLACEMENT_3D('',#4448,#3657,#3658);
#3002=AXIS2_PLACEMENT_3D('',#4454,#3662,#3663);
#3003=AXIS2_PLACEMENT_3D('',#4460,#3667,#3668);
#3004=AXIS2_PLACEMENT_3D('',#4466,#3672,#3673);
#3005=AXIS2_PLACEMENT_3D('',#4472,#3677,#3678);
#3006=AXIS2_PLACEMENT_3D('',#4478,#3682,#3683);
#3007=AXIS2_PLACEMENT_3D('',#4484,#3687,#3688);
#3008=AXIS2_PLACEMENT_3D('',#4487,#3691,#3692);
#3009=AXIS2_PLACEMENT_3D('',#4488,#3693,#3694);
#3010=AXIS2_PLACEMENT_3D('',#4489,#3695,#3696);
#3011=AXIS2_PLACEMENT_3D('',#4490,#3697,#3698);
#3012=AXIS2_PLACEMENT_3D('',#4492,#3699,#3700);
#3013=AXIS2_PLACEMENT_3D('',#4495,#3702,#3703);
#3014=AXIS2_PLACEMENT_3D('',#4496,#3704,#3705);
#3015=AXIS2_PLACEMENT_3D('',#4498,#3706,#3707);
#3016=AXIS2_PLACEMENT_3D('',#4501,#3709,#3710);
#3017=AXIS2_PLACEMENT_3D('',#4502,#3711,#3712);
#3018=AXIS2_PLACEMENT_3D('',#4503,#3713,#3714);
#3019=AXIS2_PLACEMENT_3D('',#4504,#3715,#3716);
#3020=AXIS2_PLACEMENT_3D('',#4505,#3717,#3718);
#3021=AXIS2_PLACEMENT_3D('',#4507,#3719,#3720);
#3022=AXIS2_PLACEMENT_3D('',#4510,#3722,#3723);
#3023=AXIS2_PLACEMENT_3D('',#4511,#3724,#3725);
#3024=AXIS2_PLACEMENT_3D('',#4513,#3726,#3727);
#3025=AXIS2_PLACEMENT_3D('',#4516,#3729,#3730);
#3026=AXIS2_PLACEMENT_3D('',#4517,#3731,#3732);
#3027=AXIS2_PLACEMENT_3D('',#4518,#3733,#3734);
#3028=AXIS2_PLACEMENT_3D('',#4519,#3735,#3736);
#3029=AXIS2_PLACEMENT_3D('',#4520,#3737,#3738);
#3030=AXIS2_PLACEMENT_3D('',#4522,#3739,#3740);
#3031=AXIS2_PLACEMENT_3D('',#4525,#3742,#3743);
#3032=AXIS2_PLACEMENT_3D('',#4526,#3744,#3745);
#3033=AXIS2_PLACEMENT_3D('',#4528,#3746,#3747);
#3034=AXIS2_PLACEMENT_3D('',#4531,#3749,#3750);
#3035=AXIS2_PLACEMENT_3D('',#4532,#3751,#3752);
#3036=AXIS2_PLACEMENT_3D('',#4533,#3753,#3754);
#3037=AXIS2_PLACEMENT_3D('',#4534,#3755,#3756);
#3038=AXIS2_PLACEMENT_3D('',#4535,#3757,#3758);
#3039=AXIS2_PLACEMENT_3D('',#4537,#3759,#3760);
#3040=AXIS2_PLACEMENT_3D('',#4540,#3762,#3763);
#3041=AXIS2_PLACEMENT_3D('',#4541,#3764,#3765);
#3042=AXIS2_PLACEMENT_3D('',#4543,#3766,#3767);
#3043=AXIS2_PLACEMENT_3D('',#4546,#3769,#3770);
#3044=AXIS2_PLACEMENT_3D('',#4547,#3771,#3772);
#3045=AXIS2_PLACEMENT_3D('',#4548,#3773,#3774);
#3046=AXIS2_PLACEMENT_3D('',#4549,#3775,#3776);
#3047=AXIS2_PLACEMENT_3D('',#4550,#3777,#3778);
#3048=AXIS2_PLACEMENT_3D('',#4552,#3779,#3780);
#3049=AXIS2_PLACEMENT_3D('',#4555,#3782,#3783);
#3050=AXIS2_PLACEMENT_3D('',#4556,#3784,#3785);
#3051=AXIS2_PLACEMENT_3D('',#4558,#3786,#3787);
#3052=AXIS2_PLACEMENT_3D('',#4561,#3789,#3790);
#3053=AXIS2_PLACEMENT_3D('',#4562,#3791,#3792);
#3054=AXIS2_PLACEMENT_3D('',#4563,#3793,#3794);
#3055=AXIS2_PLACEMENT_3D('',#4564,#3795,#3796);
#3056=AXIS2_PLACEMENT_3D('',#4565,#3797,#3798);
#3057=AXIS2_PLACEMENT_3D('',#4574,#3803,#3804);
#3058=AXIS2_PLACEMENT_3D('',#4583,#3809,#3810);
#3059=AXIS2_PLACEMENT_3D('',#4584,#3811,#3812);
#3060=AXIS2_PLACEMENT_3D('',#4585,#3813,#3814);
#3061=AXIS2_PLACEMENT_3D('',#4586,#3815,#3816);
#3062=AXIS2_PLACEMENT_3D('',#4587,#3817,#3818);
#3063=AXIS2_PLACEMENT_3D('',#4588,#3819,#3820);
#3064=AXIS2_PLACEMENT_3D('',#4589,#3821,#3822);
#3065=AXIS2_PLACEMENT_3D('',#4590,#3823,#3824);
#3066=AXIS2_PLACEMENT_3D('',#4591,#3825,#3826);
#3067=AXIS2_PLACEMENT_3D('',#4592,#3827,#3828);
#3068=AXIS2_PLACEMENT_3D('',#4593,#3829,#3830);
#3069=AXIS2_PLACEMENT_3D('',#4594,#3831,#3832);
#3070=AXIS2_PLACEMENT_3D('',#4595,#3833,#3834);
#3071=AXIS2_PLACEMENT_3D('',#4596,#3835,#3836);
#3072=AXIS2_PLACEMENT_3D('',#4597,#3837,#3838);
#3073=AXIS2_PLACEMENT_3D('',#4598,#3839,#3840);
#3074=AXIS2_PLACEMENT_3D('',#4599,#3841,#3842);
#3075=AXIS2_PLACEMENT_3D('',#4600,#3843,#3844);
#3076=AXIS2_PLACEMENT_3D('',#4601,#3845,#3846);
#3077=AXIS2_PLACEMENT_3D('',#4602,#3847,#3848);
#3078=AXIS2_PLACEMENT_3D('',#4603,#3849,#3850);
#3079=AXIS2_PLACEMENT_3D('',#4604,#3851,#3852);
#3080=AXIS2_PLACEMENT_3D('',#4605,#3853,#3854);
#3081=AXIS2_PLACEMENT_3D('',#4606,#3855,#3856);
#3082=AXIS2_PLACEMENT_3D('',#4607,#3857,#3858);
#3083=AXIS2_PLACEMENT_3D('',#4608,#3859,#3860);
#3084=AXIS2_PLACEMENT_3D('',#4609,#3861,#3862);
#3085=AXIS2_PLACEMENT_3D('',#4610,#3863,#3864);
#3086=AXIS2_PLACEMENT_3D('',#4611,#3865,#3866);
#3087=DIRECTION('axis',(0.,0.,1.));
#3088=DIRECTION('refdir',(1.,0.,0.));
#3089=DIRECTION('axis',(0.,0.,1.));
#3090=DIRECTION('refdir',(1.,0.,0.));
#3091=DIRECTION('center_axis',(0.,0.,-1.));
#3092=DIRECTION('ref_axis',(1.,0.,0.));
#3093=DIRECTION('center_axis',(0.,0.,-1.));
#3094=DIRECTION('ref_axis',(1.,0.,0.));
#3095=DIRECTION('',(0.,0.,-1.));
#3096=DIRECTION('center_axis',(0.,0.,1.));
#3097=DIRECTION('ref_axis',(1.,0.,0.));
#3098=DIRECTION('center_axis',(0.,0.,-1.));
#3099=DIRECTION('ref_axis',(1.,0.,0.));
#3100=DIRECTION('center_axis',(0.,0.,-1.));
#3101=DIRECTION('ref_axis',(1.,0.,0.));
#3102=DIRECTION('',(0.,0.,-1.));
#3103=DIRECTION('center_axis',(0.,0.,1.));
#3104=DIRECTION('ref_axis',(1.,0.,0.));
#3105=DIRECTION('center_axis',(0.,1.,0.));
#3106=DIRECTION('ref_axis',(0.,0.,-1.));
#3107=DIRECTION('center_axis',(0.,-1.,0.));
#3108=DIRECTION('ref_axis',(0.,0.,-1.));
#3109=DIRECTION('',(0.,1.,0.));
#3110=DIRECTION('center_axis',(0.,-1.,0.));
#3111=DIRECTION('ref_axis',(0.,0.,-1.));
#3112=DIRECTION('center_axis',(0.,1.,0.));
#3113=DIRECTION('ref_axis',(0.,0.,-1.));
#3114=DIRECTION('center_axis',(0.,-1.,0.));
#3115=DIRECTION('ref_axis',(0.,0.,-1.));
#3116=DIRECTION('',(0.,1.,0.));
#3117=DIRECTION('center_axis',(0.,-1.,0.));
#3118=DIRECTION('ref_axis',(0.,0.,-1.));
#3119=DIRECTION('center_axis',(0.,1.,0.));
#3120=DIRECTION('ref_axis',(0.,0.,-1.));
#3121=DIRECTION('center_axis',(0.,-1.,0.));
#3122=DIRECTION('ref_axis',(0.,0.,-1.));
#3123=DIRECTION('',(0.,1.,0.));
#3124=DIRECTION('center_axis',(0.,-1.,0.));
#3125=DIRECTION('ref_axis',(0.,0.,-1.));
#3126=DIRECTION('center_axis',(0.,1.,0.));
#3127=DIRECTION('ref_axis',(0.,0.,-1.));
#3128=DIRECTION('center_axis',(0.,-1.,0.));
#3129=DIRECTION('ref_axis',(0.,0.,-1.));
#3130=DIRECTION('',(0.,1.,0.));
#3131=DIRECTION('center_axis',(0.,-1.,0.));
#3132=DIRECTION('ref_axis',(0.,0.,-1.));
#3133=DIRECTION('center_axis',(0.,1.,0.));
#3134=DIRECTION('ref_axis',(-1.,0.,0.));
#3135=DIRECTION('',(1.,0.,0.));
#3136=DIRECTION('',(0.,0.,1.));
#3137=DIRECTION('',(-1.,0.,0.));
#3138=DIRECTION('',(0.,0.,1.));
#3139=DIRECTION('center_axis',(0.,1.,0.));
#3140=DIRECTION('ref_axis',(-1.,0.,0.));
#3141=DIRECTION('',(1.,0.,0.));
#3142=DIRECTION('',(0.,0.,1.));
#3143=DIRECTION('',(-1.,0.,0.));
#3144=DIRECTION('',(0.,0.,1.));
#3145=DIRECTION('center_axis',(0.,-1.,0.));
#3146=DIRECTION('ref_axis',(1.,0.,0.));
#3147=DIRECTION('',(1.,0.,0.));
#3148=DIRECTION('',(0.,0.,1.));
#3149=DIRECTION('',(-1.,0.,0.));
#3150=DIRECTION('',(0.,0.,-1.));
#3151=DIRECTION('center_axis',(0.,0.,1.));
#3152=DIRECTION('ref_axis',(1.,0.,0.));
#3153=DIRECTION('',(0.,-1.,0.));
#3154=DIRECTION('',(0.,1.,0.));
#3155=DIRECTION('center_axis',(0.,0.,1.));
#3156=DIRECTION('ref_axis',(1.,0.,0.));
#3157=DIRECTION('',(0.,-1.,0.));
#3158=DIRECTION('',(0.,1.,0.));
#3159=DIRECTION('center_axis',(0.,1.,0.));
#3160=DIRECTION('ref_axis',(-1.,0.,0.));
#3161=DIRECTION('',(1.,0.,0.));
#3162=DIRECTION('',(0.,0.,1.));
#3163=DIRECTION('',(1.,0.,0.));
#3164=DIRECTION('',(0.,0.,-1.));
#3165=DIRECTION('center_axis',(1.,0.,0.));
#3166=DIRECTION('ref_axis',(0.,1.,0.));
#3167=DIRECTION('',(0.,1.,0.));
#3168=DIRECTION('',(0.,1.,0.));
#3169=DIRECTION('center_axis',(-1.,0.,0.));
#3170=DIRECTION('ref_axis',(0.,-1.,0.));
#3171=DIRECTION('',(0.,-1.,0.));
#3172=DIRECTION('',(0.,-1.,0.));
#3173=DIRECTION('center_axis',(0.,0.,1.));
#3174=DIRECTION('ref_axis',(1.,0.,0.));
#3175=DIRECTION('center_axis',(0.,0.,1.));
#3176=DIRECTION('ref_axis',(1.,0.,0.));
#3177=DIRECTION('axis',(0.,0.,1.));
#3178=DIRECTION('refdir',(1.,0.,0.));
#3179=DIRECTION('center_axis',(0.,0.,-1.));
#3180=DIRECTION('ref_axis',(1.,0.,0.));
#3181=DIRECTION('center_axis',(0.,0.,-1.));
#3182=DIRECTION('ref_axis',(1.,0.,0.));
#3183=DIRECTION('',(0.,0.,-1.));
#3184=DIRECTION('center_axis',(0.,0.,1.));
#3185=DIRECTION('ref_axis',(1.,0.,0.));
#3186=DIRECTION('center_axis',(-0.309016994374948,-0.951056516295153,0.));
#3187=DIRECTION('ref_axis',(0.951056516295153,-0.309016994374948,0.));
#3188=DIRECTION('',(0.951056516295153,-0.309016994374948,0.));
#3189=DIRECTION('',(0.,0.,1.));
#3190=DIRECTION('',(0.951056516295153,-0.309016994374948,0.));
#3191=DIRECTION('',(0.,0.,1.));
#3192=DIRECTION('center_axis',(0.990144448700884,0.140049886493426,0.));
#3193=DIRECTION('ref_axis',(-0.140049886493426,0.990144448700885,0.));
#3194=DIRECTION('',(-0.140049886493426,0.990144448700885,0.));
#3195=DIRECTION('',(-0.140049886493426,0.990144448700885,0.));
#3196=DIRECTION('',(0.,0.,1.));
#3197=DIRECTION('center_axis',(-0.587785252292474,-0.809016994374947,0.));
#3198=DIRECTION('ref_axis',(0.809016994374947,-0.587785252292473,0.));
#3199=DIRECTION('',(0.809016994374947,-0.587785252292473,0.));
#3200=DIRECTION('',(0.809016994374947,-0.587785252292473,0.));
#3201=DIRECTION('',(0.,0.,1.));
#3202=DIRECTION('center_axis',(0.9849611249972,-0.172776104378617,0.));
#3203=DIRECTION('ref_axis',(0.172776104378617,0.9849611249972,0.));
#3204=DIRECTION('',(0.172776104378617,0.9849611249972,0.));
#3205=DIRECTION('',(0.172776104378617,0.9849611249972,0.));
#3206=DIRECTION('',(0.,0.,1.));
#3207=DIRECTION('center_axis',(-0.809016994374948,-0.587785252292473,0.));
#3208=DIRECTION('ref_axis',(0.587785252292473,-0.809016994374948,0.));
#3209=DIRECTION('',(0.587785252292473,-0.809016994374948,0.));
#3210=DIRECTION('',(0.587785252292473,-0.809016994374948,0.));
#3211=DIRECTION('',(0.,0.,1.));
#3212=DIRECTION('center_axis',(0.8833629437511,-0.468689566352177,0.));
#3213=DIRECTION('ref_axis',(0.468689566352177,0.8833629437511,0.));
#3214=DIRECTION('',(0.468689566352177,0.8833629437511,0.));
#3215=DIRECTION('',(0.468689566352177,0.8833629437511,0.));
#3216=DIRECTION('',(0.,0.,1.));
#3217=DIRECTION('center_axis',(-0.951056516295154,-0.309016994374947,0.));
#3218=DIRECTION('ref_axis',(0.309016994374947,-0.951056516295154,0.));
#3219=DIRECTION('',(0.309016994374947,-0.951056516295154,0.));
#3220=DIRECTION('',(0.309016994374947,-0.951056516295154,0.));
#3221=DIRECTION('',(0.,0.,1.));
#3222=DIRECTION('center_axis',(0.695295042819105,-0.718724428018958,0.));
#3223=DIRECTION('ref_axis',(0.718724428018958,0.695295042819105,0.));
#3224=DIRECTION('',(0.718724428018958,0.695295042819105,0.));
#3225=DIRECTION('',(0.718724428018958,0.695295042819105,0.));
#3226=DIRECTION('',(0.,0.,1.));
#3227=DIRECTION('center_axis',(-1.,1.83697019872103E-16,0.));
#3228=DIRECTION('ref_axis',(-1.83697019872103E-16,-1.,0.));
#3229=DIRECTION('',(-1.83697019872103E-16,-1.,0.));
#3230=DIRECTION('',(-1.83697019872103E-16,-1.,0.));
#3231=DIRECTION('',(0.,0.,1.));
#3232=DIRECTION('center_axis',(0.439166818690556,-0.898405535023698,0.));
#3233=DIRECTION('ref_axis',(0.898405535023697,0.439166818690556,0.));
#3234=DIRECTION('',(0.898405535023697,0.439166818690556,0.));
#3235=DIRECTION('',(0.898405535023697,0.439166818690556,0.));
#3236=DIRECTION('',(0.,0.,1.));
#3237=DIRECTION('center_axis',(-0.951056516295154,0.309016994374948,0.));
#3238=DIRECTION('ref_axis',(-0.309016994374948,-0.951056516295153,0.));
#3239=DIRECTION('',(-0.309016994374948,-0.951056516295153,0.));
#3240=DIRECTION('',(-0.309016994374948,-0.951056516295153,0.));
#3241=DIRECTION('',(0.,0.,1.));
#3242=DIRECTION('center_axis',(0.140049886493426,-0.990144448700884,0.));
#3243=DIRECTION('ref_axis',(0.990144448700885,0.140049886493426,0.));
#3244=DIRECTION('',(0.990144448700885,0.140049886493426,0.));
#3245=DIRECTION('',(0.990144448700885,0.140049886493426,0.));
#3246=DIRECTION('',(0.,0.,1.));
#3247=DIRECTION('center_axis',(-0.809016994374947,0.587785252292473,0.));
#3248=DIRECTION('ref_axis',(-0.587785252292473,-0.809016994374947,0.));
#3249=DIRECTION('',(-0.587785252292473,-0.809016994374947,0.));
#3250=DIRECTION('',(-0.587785252292473,-0.809016994374947,0.));
#3251=DIRECTION('',(0.,0.,1.));
#3252=DIRECTION('center_axis',(-0.172776104378617,-0.9849611249972,0.));
#3253=DIRECTION('ref_axis',(0.9849611249972,-0.172776104378617,0.));
#3254=DIRECTION('',(0.9849611249972,-0.172776104378617,0.));
#3255=DIRECTION('',(0.9849611249972,-0.172776104378617,0.));
#3256=DIRECTION('',(0.,0.,1.));
#3257=DIRECTION('center_axis',(-0.587785252292473,0.809016994374948,0.));
#3258=DIRECTION('ref_axis',(-0.809016994374947,-0.587785252292473,0.));
#3259=DIRECTION('',(-0.809016994374947,-0.587785252292473,0.));
#3260=DIRECTION('',(-0.809016994374947,-0.587785252292473,0.));
#3261=DIRECTION('',(0.,0.,1.));
#3262=DIRECTION('center_axis',(-0.468689566352177,-0.8833629437511,0.));
#3263=DIRECTION('ref_axis',(0.8833629437511,-0.468689566352176,0.));
#3264=DIRECTION('',(0.8833629437511,-0.468689566352176,0.));
#3265=DIRECTION('',(0.8833629437511,-0.468689566352176,0.));
#3266=DIRECTION('',(0.,0.,1.));
#3267=DIRECTION('center_axis',(-0.309016994374947,0.951056516295154,0.));
#3268=DIRECTION('ref_axis',(-0.951056516295154,-0.309016994374947,0.));
#3269=DIRECTION('',(-0.951056516295154,-0.309016994374947,0.));
#3270=DIRECTION('',(-0.951056516295154,-0.309016994374947,0.));
#3271=DIRECTION('',(0.,0.,1.));
#3272=DIRECTION('center_axis',(-0.718724428018958,-0.695295042819105,0.));
#3273=DIRECTION('ref_axis',(0.695295042819105,-0.718724428018958,0.));
#3274=DIRECTION('',(0.695295042819105,-0.718724428018958,0.));
#3275=DIRECTION('',(0.695295042819105,-0.718724428018958,0.));
#3276=DIRECTION('',(0.,0.,1.));
#3277=DIRECTION('center_axis',(1.22464679914735E-16,1.,0.));
#3278=DIRECTION('ref_axis',(-1.,1.22464679914735E-16,0.));
#3279=DIRECTION('',(-1.,1.22464679914735E-16,0.));
#3280=DIRECTION('',(-1.,1.22464679914735E-16,0.));
#3281=DIRECTION('',(0.,0.,1.));
#3282=DIRECTION('center_axis',(-0.898405535023698,-0.439166818690556,0.));
#3283=DIRECTION('ref_axis',(0.439166818690556,-0.898405535023697,0.));
#3284=DIRECTION('',(0.439166818690556,-0.898405535023697,0.));
#3285=DIRECTION('',(0.439166818690556,-0.898405535023697,0.));
#3286=DIRECTION('',(0.,0.,1.));
#3287=DIRECTION('center_axis',(0.309016994374948,0.951056516295154,0.));
#3288=DIRECTION('ref_axis',(-0.951056516295153,0.309016994374948,0.));
#3289=DIRECTION('',(-0.951056516295153,0.309016994374948,0.));
#3290=DIRECTION('',(-0.951056516295153,0.309016994374948,0.));
#3291=DIRECTION('',(0.,0.,1.));
#3292=DIRECTION('center_axis',(-0.990144448700884,-0.140049886493426,0.));
#3293=DIRECTION('ref_axis',(0.140049886493426,-0.990144448700885,0.));
#3294=DIRECTION('',(0.140049886493426,-0.990144448700885,0.));
#3295=DIRECTION('',(0.140049886493426,-0.990144448700885,0.));
#3296=DIRECTION('',(0.,0.,1.));
#3297=DIRECTION('center_axis',(0.587785252292473,0.809016994374947,0.));
#3298=DIRECTION('ref_axis',(-0.809016994374947,0.587785252292473,0.));
#3299=DIRECTION('',(-0.809016994374947,0.587785252292473,0.));
#3300=DIRECTION('',(-0.809016994374947,0.587785252292473,0.));
#3301=DIRECTION('',(0.,0.,1.));
#3302=DIRECTION('center_axis',(-0.9849611249972,0.172776104378617,0.));
#3303=DIRECTION('ref_axis',(-0.172776104378617,-0.9849611249972,0.));
#3304=DIRECTION('',(-0.172776104378617,-0.9849611249972,0.));
#3305=DIRECTION('',(-0.172776104378617,-0.9849611249972,0.));
#3306=DIRECTION('',(0.,0.,1.));
#3307=DIRECTION('center_axis',(0.809016994374948,0.587785252292473,0.));
#3308=DIRECTION('ref_axis',(-0.587785252292473,0.809016994374947,0.));
#3309=DIRECTION('',(-0.587785252292473,0.809016994374947,0.));
#3310=DIRECTION('',(-0.587785252292473,0.809016994374947,0.));
#3311=DIRECTION('',(0.,0.,1.));
#3312=DIRECTION('center_axis',(-0.8833629437511,0.468689566352176,0.));
#3313=DIRECTION('ref_axis',(-0.468689566352176,-0.8833629437511,0.));
#3314=DIRECTION('',(-0.468689566352176,-0.8833629437511,0.));
#3315=DIRECTION('',(-0.468689566352176,-0.8833629437511,0.));
#3316=DIRECTION('',(0.,0.,1.));
#3317=DIRECTION('center_axis',(0.951056516295154,0.309016994374947,0.));
#3318=DIRECTION('ref_axis',(-0.309016994374947,0.951056516295154,0.));
#3319=DIRECTION('',(-0.309016994374947,0.951056516295154,0.));
#3320=DIRECTION('',(-0.309016994374947,0.951056516295154,0.));
#3321=DIRECTION('',(0.,0.,1.));
#3322=DIRECTION('center_axis',(-0.695295042819106,0.718724428018958,0.));
#3323=DIRECTION('ref_axis',(-0.718724428018958,-0.695295042819106,0.));
#3324=DIRECTION('',(-0.718724428018958,-0.695295042819105,0.));
#3325=DIRECTION('',(-0.718724428018958,-0.695295042819105,0.));
#3326=DIRECTION('',(0.,0.,1.));
#3327=DIRECTION('center_axis',(1.,-6.12323399573677E-17,0.));
#3328=DIRECTION('ref_axis',(6.12323399573677E-17,1.,0.));
#3329=DIRECTION('',(6.12323399573677E-17,1.,0.));
#3330=DIRECTION('',(6.12323399573677E-17,1.,0.));
#3331=DIRECTION('',(0.,0.,1.));
#3332=DIRECTION('center_axis',(-0.439166818690556,0.898405535023698,0.));
#3333=DIRECTION('ref_axis',(-0.898405535023697,-0.439166818690556,0.));
#3334=DIRECTION('',(-0.898405535023697,-0.439166818690556,0.));
#3335=DIRECTION('',(-0.898405535023697,-0.439166818690556,0.));
#3336=DIRECTION('',(0.,0.,1.));
#3337=DIRECTION('center_axis',(0.951056516295154,-0.309016994374948,0.));
#3338=DIRECTION('ref_axis',(0.309016994374948,0.951056516295153,0.));
#3339=DIRECTION('',(0.309016994374948,0.951056516295153,0.));
#3340=DIRECTION('',(0.309016994374948,0.951056516295153,0.));
#3341=DIRECTION('',(0.,0.,1.));
#3342=DIRECTION('center_axis',(-0.140049886493427,0.990144448700884,0.));
#3343=DIRECTION('ref_axis',(-0.990144448700884,-0.140049886493427,0.));
#3344=DIRECTION('',(-0.990144448700884,-0.140049886493427,0.));
#3345=DIRECTION('',(-0.990144448700884,-0.140049886493427,0.));
#3346=DIRECTION('',(0.,0.,1.));
#3347=DIRECTION('center_axis',(0.809016994374948,-0.587785252292473,0.));
#3348=DIRECTION('ref_axis',(0.587785252292473,0.809016994374947,0.));
#3349=DIRECTION('',(0.587785252292473,0.809016994374947,0.));
#3350=DIRECTION('',(0.587785252292473,0.809016994374947,0.));
#3351=DIRECTION('',(0.,0.,1.));
#3352=DIRECTION('center_axis',(0.172776104378617,0.9849611249972,0.));
#3353=DIRECTION('ref_axis',(-0.9849611249972,0.172776104378617,0.));
#3354=DIRECTION('',(-0.9849611249972,0.172776104378617,0.));
#3355=DIRECTION('',(-0.9849611249972,0.172776104378617,0.));
#3356=DIRECTION('',(0.,0.,1.));
#3357=DIRECTION('center_axis',(0.587785252292473,-0.809016994374948,0.));
#3358=DIRECTION('ref_axis',(0.809016994374947,0.587785252292473,0.));
#3359=DIRECTION('',(0.809016994374947,0.587785252292473,0.));
#3360=DIRECTION('',(0.809016994374947,0.587785252292473,0.));
#3361=DIRECTION('',(0.,0.,1.));
#3362=DIRECTION('center_axis',(0.468689566352177,0.8833629437511,0.));
#3363=DIRECTION('ref_axis',(-0.8833629437511,0.468689566352177,0.));
#3364=DIRECTION('',(-0.8833629437511,0.468689566352177,0.));
#3365=DIRECTION('',(-0.8833629437511,0.468689566352177,0.));
#3366=DIRECTION('',(0.,0.,1.));
#3367=DIRECTION('center_axis',(0.309016994374948,-0.951056516295154,0.));
#3368=DIRECTION('ref_axis',(0.951056516295153,0.309016994374948,0.));
#3369=DIRECTION('',(0.951056516295153,0.309016994374948,0.));
#3370=DIRECTION('',(0.951056516295153,0.309016994374948,0.));
#3371=DIRECTION('',(0.,0.,1.));
#3372=DIRECTION('center_axis',(0.718724428018958,0.695295042819106,0.));
#3373=DIRECTION('ref_axis',(-0.695295042819106,0.718724428018958,0.));
#3374=DIRECTION('',(-0.695295042819106,0.718724428018958,0.));
#3375=DIRECTION('',(-0.695295042819106,0.718724428018958,0.));
#3376=DIRECTION('',(0.,0.,1.));
#3377=DIRECTION('center_axis',(0.,-1.,0.));
#3378=DIRECTION('ref_axis',(1.,0.,0.));
#3379=DIRECTION('',(1.,0.,0.));
#3380=DIRECTION('',(1.,0.,0.));
#3381=DIRECTION('',(0.,0.,1.));
#3382=DIRECTION('center_axis',(0.898405535023698,0.439166818690556,0.));
#3383=DIRECTION('ref_axis',(-0.439166818690556,0.898405535023698,0.));
#3384=DIRECTION('',(-0.439166818690556,0.898405535023698,0.));
#3385=DIRECTION('',(-0.439166818690556,0.898405535023698,0.));
#3386=DIRECTION('center_axis',(0.,0.,1.));
#3387=DIRECTION('ref_axis',(1.,0.,0.));
#3388=DIRECTION('center_axis',(0.,0.,1.));
#3389=DIRECTION('ref_axis',(1.,0.,0.));
#3390=DIRECTION('axis',(0.,0.,1.));
#3391=DIRECTION('refdir',(1.,0.,0.));
#3392=DIRECTION('center_axis',(0.,0.,-1.));
#3393=DIRECTION('ref_axis',(1.,0.,0.));
#3394=DIRECTION('center_axis',(0.,0.,-1.));
#3395=DIRECTION('ref_axis',(1.,0.,0.));
#3396=DIRECTION('',(0.,0.,-1.));
#3397=DIRECTION('center_axis',(0.,0.,1.));
#3398=DIRECTION('ref_axis',(1.,0.,0.));
#3399=DIRECTION('center_axis',(0.,0.,-1.));
#3400=DIRECTION('ref_axis',(1.,0.,0.));
#3401=DIRECTION('center_axis',(0.,0.,-1.));
#3402=DIRECTION('ref_axis',(1.,0.,0.));
#3403=DIRECTION('',(0.,0.,-1.));
#3404=DIRECTION('center_axis',(0.,0.,1.));
#3405=DIRECTION('ref_axis',(1.,0.,0.));
#3406=DIRECTION('center_axis',(0.,0.,-1.));
#3407=DIRECTION('ref_axis',(1.,0.,0.));
#3408=DIRECTION('center_axis',(0.,0.,-1.));
#3409=DIRECTION('ref_axis',(1.,0.,0.));
#3410=DIRECTION('',(0.,0.,-1.));
#3411=DIRECTION('center_axis',(0.,0.,1.));
#3412=DIRECTION('ref_axis',(1.,0.,0.));
#3413=DIRECTION('center_axis',(-1.,0.,0.));
#3414=DIRECTION('ref_axis',(0.,-1.,0.));
#3415=DIRECTION('',(0.,-1.,0.));
#3416=DIRECTION('',(0.,0.,1.));
#3417=DIRECTION('',(0.,-1.,0.));
#3418=DIRECTION('',(0.,0.,1.));
#3419=DIRECTION('center_axis',(-0.707106781186548,0.707106781186548,0.));
#3420=DIRECTION('ref_axis',(-0.707106781186548,-0.707106781186548,0.));
#3421=DIRECTION('',(-0.707106781186547,-0.707106781186547,0.));
#3422=DIRECTION('',(-0.707106781186547,-0.707106781186547,0.));
#3423=DIRECTION('',(0.,0.,1.));
#3424=DIRECTION('center_axis',(0.,1.,0.));
#3425=DIRECTION('ref_axis',(-1.,0.,0.));
#3426=DIRECTION('',(-1.,0.,0.));
#3427=DIRECTION('',(-1.,0.,0.));
#3428=DIRECTION('',(0.,0.,1.));
#3429=DIRECTION('center_axis',(0.707106781186548,0.707106781186548,0.));
#3430=DIRECTION('ref_axis',(-0.707106781186548,0.707106781186548,0.));
#3431=DIRECTION('',(-0.707106781186547,0.707106781186547,0.));
#3432=DIRECTION('',(-0.707106781186547,0.707106781186547,0.));
#3433=DIRECTION('',(0.,0.,1.));
#3434=DIRECTION('center_axis',(1.,0.,0.));
#3435=DIRECTION('ref_axis',(0.,1.,0.));
#3436=DIRECTION('',(0.,1.,0.));
#3437=DIRECTION('',(0.,1.,0.));
#3438=DIRECTION('',(0.,0.,1.));
#3439=DIRECTION('center_axis',(0.707106781186548,-0.707106781186548,0.));
#3440=DIRECTION('ref_axis',(0.707106781186548,0.707106781186548,0.));
#3441=DIRECTION('',(0.707106781186547,0.707106781186547,0.));
#3442=DIRECTION('',(0.707106781186547,0.707106781186547,0.));
#3443=DIRECTION('',(0.,0.,1.));
#3444=DIRECTION('center_axis',(0.,-1.,0.));
#3445=DIRECTION('ref_axis',(1.,0.,0.));
#3446=DIRECTION('',(1.,0.,0.));
#3447=DIRECTION('',(1.,0.,0.));
#3448=DIRECTION('',(0.,0.,1.));
#3449=DIRECTION('center_axis',(-0.707106781186548,-0.707106781186548,0.));
#3450=DIRECTION('ref_axis',(0.707106781186548,-0.707106781186548,0.));
#3451=DIRECTION('',(0.707106781186547,-0.707106781186547,0.));
#3452=DIRECTION('',(0.707106781186547,-0.707106781186547,0.));
#3453=DIRECTION('center_axis',(0.,0.,1.));
#3454=DIRECTION('ref_axis',(1.,0.,0.));
#3455=DIRECTION('center_axis',(0.,0.,1.));
#3456=DIRECTION('ref_axis',(1.,0.,0.));
#3457=DIRECTION('axis',(0.,0.,1.));
#3458=DIRECTION('refdir',(1.,0.,0.));
#3459=DIRECTION('center_axis',(0.,0.,1.));
#3460=DIRECTION('ref_axis',(1.,0.,0.));
#3461=DIRECTION('center_axis',(0.,0.,1.));
#3462=DIRECTION('ref_axis',(1.,0.,0.));
#3463=DIRECTION('',(0.,0.,1.));
#3464=DIRECTION('center_axis',(0.,0.,1.));
#3465=DIRECTION('ref_axis',(1.,0.,0.));
#3466=DIRECTION('center_axis',(0.,0.,-1.));
#3467=DIRECTION('ref_axis',(-1.,0.,0.));
#3468=DIRECTION('center_axis',(0.,0.,-1.));
#3469=DIRECTION('ref_axis',(1.,0.,0.));
#3470=DIRECTION('center_axis',(0.,0.,1.));
#3471=DIRECTION('ref_axis',(1.,0.,0.));
#3472=DIRECTION('center_axis',(0.,0.,1.));
#3473=DIRECTION('ref_axis',(1.,0.,0.));
#3474=DIRECTION('center_axis',(0.,0.,1.));
#3475=DIRECTION('ref_axis',(1.,0.,0.));
#3476=DIRECTION('center_axis',(0.,0.,1.));
#3477=DIRECTION('ref_axis',(1.,0.,0.));
#3478=DIRECTION('',(0.,0.,-1.));
#3479=DIRECTION('center_axis',(0.,0.,1.));
#3480=DIRECTION('ref_axis',(1.,0.,0.));
#3481=DIRECTION('center_axis',(0.,0.,1.));
#3482=DIRECTION('ref_axis',(1.,0.,0.));
#3483=DIRECTION('center_axis',(0.,0.,1.));
#3484=DIRECTION('ref_axis',(1.,0.,0.));
#3485=DIRECTION('center_axis',(0.,0.,1.));
#3486=DIRECTION('ref_axis',(1.,0.,0.));
#3487=DIRECTION('',(0.,0.,-1.));
#3488=DIRECTION('center_axis',(0.,0.,1.));
#3489=DIRECTION('ref_axis',(1.,0.,0.));
#3490=DIRECTION('center_axis',(0.,0.,1.));
#3491=DIRECTION('ref_axis',(1.,0.,0.));
#3492=DIRECTION('center_axis',(0.,0.,1.));
#3493=DIRECTION('ref_axis',(1.,0.,0.));
#3494=DIRECTION('',(0.,0.,-1.));
#3495=DIRECTION('center_axis',(0.,0.,1.));
#3496=DIRECTION('ref_axis',(1.,0.,0.));
#3497=DIRECTION('axis',(0.,0.,1.));
#3498=DIRECTION('refdir',(1.,0.,0.));
#3499=DIRECTION('center_axis',(0.,0.,1.));
#3500=DIRECTION('ref_axis',(1.,0.,0.));
#3501=DIRECTION('center_axis',(0.,0.,1.));
#3502=DIRECTION('ref_axis',(1.,0.,0.));
#3503=DIRECTION('',(0.,0.,1.));
#3504=DIRECTION('center_axis',(0.,0.,1.));
#3505=DIRECTION('ref_axis',(1.,0.,0.));
#3506=DIRECTION('center_axis',(0.,0.,-1.));
#3507=DIRECTION('ref_axis',(-1.,0.,0.));
#3508=DIRECTION('center_axis',(0.,0.,-1.));
#3509=DIRECTION('ref_axis',(1.,0.,0.));
#3510=DIRECTION('center_axis',(0.,0.,1.));
#3511=DIRECTION('ref_axis',(1.,0.,0.));
#3512=DIRECTION('center_axis',(0.,0.,1.));
#3513=DIRECTION('ref_axis',(1.,0.,0.));
#3514=DIRECTION('center_axis',(0.,0.,1.));
#3515=DIRECTION('ref_axis',(1.,0.,0.));
#3516=DIRECTION('center_axis',(0.,0.,1.));
#3517=DIRECTION('ref_axis',(1.,0.,0.));
#3518=DIRECTION('',(0.,0.,-1.));
#3519=DIRECTION('center_axis',(0.,0.,1.));
#3520=DIRECTION('ref_axis',(1.,0.,0.));
#3521=DIRECTION('center_axis',(0.,0.,1.));
#3522=DIRECTION('ref_axis',(1.,0.,0.));
#3523=DIRECTION('center_axis',(0.,0.,1.));
#3524=DIRECTION('ref_axis',(1.,0.,0.));
#3525=DIRECTION('center_axis',(0.,0.,1.));
#3526=DIRECTION('ref_axis',(1.,0.,0.));
#3527=DIRECTION('',(0.,0.,-1.));
#3528=DIRECTION('center_axis',(0.,0.,1.));
#3529=DIRECTION('ref_axis',(1.,0.,0.));
#3530=DIRECTION('center_axis',(0.,0.,1.));
#3531=DIRECTION('ref_axis',(1.,0.,0.));
#3532=DIRECTION('center_axis',(0.,0.,1.));
#3533=DIRECTION('ref_axis',(1.,0.,0.));
#3534=DIRECTION('',(0.,0.,-1.));
#3535=DIRECTION('center_axis',(0.,0.,1.));
#3536=DIRECTION('ref_axis',(1.,0.,0.));
#3537=DIRECTION('axis',(0.,0.,1.));
#3538=DIRECTION('refdir',(1.,0.,0.));
#3539=DIRECTION('center_axis',(0.,0.,1.));
#3540=DIRECTION('ref_axis',(1.,0.,0.));
#3541=DIRECTION('center_axis',(0.,0.,1.));
#3542=DIRECTION('ref_axis',(1.,0.,0.));
#3543=DIRECTION('',(0.,0.,1.));
#3544=DIRECTION('center_axis',(0.,0.,1.));
#3545=DIRECTION('ref_axis',(1.,0.,0.));
#3546=DIRECTION('center_axis',(0.,0.,-1.));
#3547=DIRECTION('ref_axis',(-1.,0.,0.));
#3548=DIRECTION('center_axis',(0.,0.,-1.));
#3549=DIRECTION('ref_axis',(1.,0.,0.));
#3550=DIRECTION('center_axis',(0.,0.,1.));
#3551=DIRECTION('ref_axis',(1.,0.,0.));
#3552=DIRECTION('center_axis',(0.,0.,1.));
#3553=DIRECTION('ref_axis',(1.,0.,0.));
#3554=DIRECTION('center_axis',(0.,0.,1.));
#3555=DIRECTION('ref_axis',(1.,0.,0.));
#3556=DIRECTION('center_axis',(0.,0.,1.));
#3557=DIRECTION('ref_axis',(1.,0.,0.));
#3558=DIRECTION('',(0.,0.,-1.));
#3559=DIRECTION('center_axis',(0.,0.,1.));
#3560=DIRECTION('ref_axis',(1.,0.,0.));
#3561=DIRECTION('center_axis',(0.,0.,1.));
#3562=DIRECTION('ref_axis',(1.,0.,0.));
#3563=DIRECTION('center_axis',(0.,0.,1.));
#3564=DIRECTION('ref_axis',(1.,0.,0.));
#3565=DIRECTION('center_axis',(0.,0.,1.));
#3566=DIRECTION('ref_axis',(1.,0.,0.));
#3567=DIRECTION('',(0.,0.,-1.));
#3568=DIRECTION('center_axis',(0.,0.,1.));
#3569=DIRECTION('ref_axis',(1.,0.,0.));
#3570=DIRECTION('center_axis',(0.,0.,1.));
#3571=DIRECTION('ref_axis',(1.,0.,0.));
#3572=DIRECTION('center_axis',(0.,0.,1.));
#3573=DIRECTION('ref_axis',(1.,0.,0.));
#3574=DIRECTION('',(0.,0.,-1.));
#3575=DIRECTION('center_axis',(0.,0.,1.));
#3576=DIRECTION('ref_axis',(1.,0.,0.));
#3577=DIRECTION('axis',(0.,0.,1.));
#3578=DIRECTION('refdir',(1.,0.,0.));
#3579=DIRECTION('center_axis',(-1.,0.,0.));
#3580=DIRECTION('ref_axis',(0.,1.,0.));
#3581=DIRECTION('',(0.,0.,1.));
#3582=DIRECTION('',(0.,-1.,0.));
#3583=DIRECTION('',(0.,0.,-1.));
#3584=DIRECTION('',(0.,1.,0.));
#3585=DIRECTION('center_axis',(1.,0.,0.));
#3586=DIRECTION('ref_axis',(0.,-1.,0.));
#3587=DIRECTION('',(0.,0.,-1.));
#3588=DIRECTION('',(0.,-1.,0.));
#3589=DIRECTION('',(0.,0.,1.));
#3590=DIRECTION('',(0.,1.,0.));
#3591=DIRECTION('center_axis',(0.,0.,1.));
#3592=DIRECTION('ref_axis',(1.,0.,0.));
#3593=DIRECTION('center_axis',(0.,0.,1.));
#3594=DIRECTION('ref_axis',(1.,0.,0.));
#3595=DIRECTION('center_axis',(0.,0.,-1.));
#3596=DIRECTION('ref_axis',(1.,0.,0.));
#3597=DIRECTION('center_axis',(0.,0.,1.));
#3598=DIRECTION('ref_axis',(6.12323399573677E-17,-1.,0.));
#3599=DIRECTION('center_axis',(0.,0.,-1.));
#3600=DIRECTION('ref_axis',(1.,0.,0.));
#3601=DIRECTION('center_axis',(0.,0.,1.));
#3602=DIRECTION('ref_axis',(6.12323399573677E-17,-1.,0.));
#3603=DIRECTION('center_axis',(0.,0.,1.));
#3604=DIRECTION('ref_axis',(1.,0.,0.));
#3605=DIRECTION('center_axis',(0.,0.,1.));
#3606=DIRECTION('ref_axis',(1.,0.,0.));
#3607=DIRECTION('axis',(0.,0.,1.));
#3608=DIRECTION('refdir',(1.,0.,0.));
#3609=DIRECTION('center_axis',(0.,0.,-1.));
#3610=DIRECTION('ref_axis',(1.,0.,0.));
#3611=DIRECTION('center_axis',(0.,0.,-1.));
#3612=DIRECTION('ref_axis',(1.,0.,0.));
#3613=DIRECTION('',(0.,0.,-1.));
#3614=DIRECTION('center_axis',(0.,0.,1.));
#3615=DIRECTION('ref_axis',(1.,0.,0.));
#3616=DIRECTION('center_axis',(-1.,0.,0.));
#3617=DIRECTION('ref_axis',(0.,-1.,0.));
#3618=DIRECTION('',(0.,-1.,0.));
#3619=DIRECTION('',(0.,0.,1.));
#3620=DIRECTION('',(0.,-1.,0.));
#3621=DIRECTION('',(0.,0.,1.));
#3622=DIRECTION('center_axis',(-0.832050294337843,0.554700196225229,0.));
#3623=DIRECTION('ref_axis',(-0.554700196225229,-0.832050294337843,0.));
#3624=DIRECTION('',(-0.554700196225229,-0.832050294337843,0.));
#3625=DIRECTION('',(-0.554700196225229,-0.832050294337843,0.));
#3626=DIRECTION('',(0.,0.,1.));
#3627=DIRECTION('center_axis',(-1.,0.,0.));
#3628=DIRECTION('ref_axis',(0.,-1.,0.));
#3629=DIRECTION('',(0.,-1.,0.));
#3630=DIRECTION('',(0.,-1.,0.));
#3631=DIRECTION('',(0.,0.,1.));
#3632=DIRECTION('center_axis',(-0.707106781186548,0.707106781186547,0.));
#3633=DIRECTION('ref_axis',(-0.707106781186547,-0.707106781186548,0.));
#3634=DIRECTION('',(-0.707106781186547,-0.707106781186548,0.));
#3635=DIRECTION('',(-0.707106781186547,-0.707106781186548,0.));
#3636=DIRECTION('',(0.,0.,1.));
#3637=DIRECTION('center_axis',(0.,1.,0.));
#3638=DIRECTION('ref_axis',(-1.,0.,0.));
#3639=DIRECTION('',(-1.,0.,0.));
#3640=DIRECTION('',(-1.,0.,0.));
#3641=DIRECTION('',(0.,0.,1.));
#3642=DIRECTION('center_axis',(-1.,0.,0.));
#3643=DIRECTION('ref_axis',(0.,-1.,0.));
#3644=DIRECTION('',(0.,-1.,0.));
#3645=DIRECTION('',(0.,-1.,0.));
#3646=DIRECTION('',(0.,0.,1.));
#3647=DIRECTION('center_axis',(0.,1.,0.));
#3648=DIRECTION('ref_axis',(-1.,0.,0.));
#3649=DIRECTION('',(-1.,0.,0.));
#3650=DIRECTION('',(-1.,0.,0.));
#3651=DIRECTION('',(0.,0.,1.));
#3652=DIRECTION('center_axis',(1.,0.,0.));
#3653=DIRECTION('ref_axis',(0.,1.,0.));
#3654=DIRECTION('',(0.,1.,0.));
#3655=DIRECTION('',(0.,1.,0.));
#3656=DIRECTION('',(0.,0.,1.));
#3657=DIRECTION('center_axis',(0.,-1.,0.));
#3658=DIRECTION('ref_axis',(1.,0.,0.));
#3659=DIRECTION('',(1.,0.,0.));
#3660=DIRECTION('',(1.,0.,0.));
#3661=DIRECTION('',(0.,0.,1.));
#3662=DIRECTION('center_axis',(-1.,0.,0.));
#3663=DIRECTION('ref_axis',(0.,-1.,0.));
#3664=DIRECTION('',(0.,-1.,0.));
#3665=DIRECTION('',(0.,-1.,0.));
#3666=DIRECTION('',(0.,0.,1.));
#3667=DIRECTION('center_axis',(0.,-1.,0.));
#3668=DIRECTION('ref_axis',(1.,0.,0.));
#3669=DIRECTION('',(1.,0.,0.));
#3670=DIRECTION('',(1.,0.,0.));
#3671=DIRECTION('',(0.,0.,1.));
#3672=DIRECTION('center_axis',(0.64018439966448,-0.768221279597376,0.));
#3673=DIRECTION('ref_axis',(0.768221279597376,0.64018439966448,0.));
#3674=DIRECTION('',(0.768221279597376,0.64018439966448,0.));
#3675=DIRECTION('',(0.768221279597376,0.64018439966448,0.));
#3676=DIRECTION('',(0.,0.,1.));
#3677=DIRECTION('center_axis',(0.,-1.,0.));
#3678=DIRECTION('ref_axis',(1.,0.,0.));
#3679=DIRECTION('',(1.,0.,0.));
#3680=DIRECTION('',(1.,0.,0.));
#3681=DIRECTION('',(0.,0.,1.));
#3682=DIRECTION('center_axis',(-0.948683298050514,0.316227766016838,0.));
#3683=DIRECTION('ref_axis',(-0.316227766016838,-0.948683298050514,0.));
#3684=DIRECTION('',(-0.316227766016838,-0.948683298050514,0.));
#3685=DIRECTION('',(-0.316227766016838,-0.948683298050514,0.));
#3686=DIRECTION('',(0.,0.,1.));
#3687=DIRECTION('center_axis',(0.,1.,0.));
#3688=DIRECTION('ref_axis',(-1.,0.,0.));
#3689=DIRECTION('',(-1.,0.,0.));
#3690=DIRECTION('',(-1.,0.,0.));
#3691=DIRECTION('center_axis',(0.,0.,1.));
#3692=DIRECTION('ref_axis',(1.,0.,0.));
#3693=DIRECTION('center_axis',(0.,0.,1.));
#3694=DIRECTION('ref_axis',(1.,0.,0.));
#3695=DIRECTION('axis',(0.,0.,1.));
#3696=DIRECTION('refdir',(1.,0.,0.));
#3697=DIRECTION('center_axis',(0.,0.,1.));
#3698=DIRECTION('ref_axis',(1.,0.,0.));
#3699=DIRECTION('center_axis',(0.,0.,-1.));
#3700=DIRECTION('ref_axis',(1.,0.,0.));
#3701=DIRECTION('',(0.,0.,-1.));
#3702=DIRECTION('center_axis',(0.,0.,-1.));
#3703=DIRECTION('ref_axis',(1.,0.,0.));
#3704=DIRECTION('center_axis',(0.,0.,1.));
#3705=DIRECTION('ref_axis',(1.,0.,0.));
#3706=DIRECTION('center_axis',(0.,0.,1.));
#3707=DIRECTION('ref_axis',(1.,0.,0.));
#3708=DIRECTION('',(0.,0.,-1.));
#3709=DIRECTION('center_axis',(0.,0.,1.));
#3710=DIRECTION('ref_axis',(1.,0.,0.));
#3711=DIRECTION('center_axis',(0.,0.,1.));
#3712=DIRECTION('ref_axis',(1.,0.,0.));
#3713=DIRECTION('center_axis',(0.,0.,1.));
#3714=DIRECTION('ref_axis',(1.,0.,0.));
#3715=DIRECTION('axis',(0.,0.,1.));
#3716=DIRECTION('refdir',(1.,0.,0.));
#3717=DIRECTION('center_axis',(0.,0.,1.));
#3718=DIRECTION('ref_axis',(1.,0.,0.));
#3719=DIRECTION('center_axis',(0.,0.,-1.));
#3720=DIRECTION('ref_axis',(1.,0.,0.));
#3721=DIRECTION('',(0.,0.,-1.));
#3722=DIRECTION('center_axis',(0.,0.,-1.));
#3723=DIRECTION('ref_axis',(1.,0.,0.));
#3724=DIRECTION('center_axis',(0.,0.,1.));
#3725=DIRECTION('ref_axis',(1.,0.,0.));
#3726=DIRECTION('center_axis',(0.,0.,1.));
#3727=DIRECTION('ref_axis',(1.,0.,0.));
#3728=DIRECTION('',(0.,0.,-1.));
#3729=DIRECTION('center_axis',(0.,0.,1.));
#3730=DIRECTION('ref_axis',(1.,0.,0.));
#3731=DIRECTION('center_axis',(0.,0.,1.));
#3732=DIRECTION('ref_axis',(1.,0.,0.));
#3733=DIRECTION('center_axis',(0.,0.,1.));
#3734=DIRECTION('ref_axis',(1.,0.,0.));
#3735=DIRECTION('axis',(0.,0.,1.));
#3736=DIRECTION('refdir',(1.,0.,0.));
#3737=DIRECTION('center_axis',(0.,0.,1.));
#3738=DIRECTION('ref_axis',(1.,0.,0.));
#3739=DIRECTION('center_axis',(0.,0.,-1.));
#3740=DIRECTION('ref_axis',(1.,0.,0.));
#3741=DIRECTION('',(0.,0.,-1.));
#3742=DIRECTION('center_axis',(0.,0.,-1.));
#3743=DIRECTION('ref_axis',(1.,0.,0.));
#3744=DIRECTION('center_axis',(0.,0.,1.));
#3745=DIRECTION('ref_axis',(1.,0.,0.));
#3746=DIRECTION('center_axis',(0.,0.,1.));
#3747=DIRECTION('ref_axis',(1.,0.,0.));
#3748=DIRECTION('',(0.,0.,-1.));
#3749=DIRECTION('center_axis',(0.,0.,1.));
#3750=DIRECTION('ref_axis',(1.,0.,0.));
#3751=DIRECTION('center_axis',(0.,0.,1.));
#3752=DIRECTION('ref_axis',(1.,0.,0.));
#3753=DIRECTION('center_axis',(0.,0.,1.));
#3754=DIRECTION('ref_axis',(1.,0.,0.));
#3755=DIRECTION('axis',(0.,0.,1.));
#3756=DIRECTION('refdir',(1.,0.,0.));
#3757=DIRECTION('center_axis',(0.,0.,1.));
#3758=DIRECTION('ref_axis',(1.,0.,0.));
#3759=DIRECTION('center_axis',(0.,0.,-1.));
#3760=DIRECTION('ref_axis',(1.,0.,0.));
#3761=DIRECTION('',(0.,0.,-1.));
#3762=DIRECTION('center_axis',(0.,0.,-1.));
#3763=DIRECTION('ref_axis',(1.,0.,0.));
#3764=DIRECTION('center_axis',(0.,0.,1.));
#3765=DIRECTION('ref_axis',(1.,0.,0.));
#3766=DIRECTION('center_axis',(0.,0.,1.));
#3767=DIRECTION('ref_axis',(1.,0.,0.));
#3768=DIRECTION('',(0.,0.,-1.));
#3769=DIRECTION('center_axis',(0.,0.,1.));
#3770=DIRECTION('ref_axis',(1.,0.,0.));
#3771=DIRECTION('center_axis',(0.,0.,1.));
#3772=DIRECTION('ref_axis',(1.,0.,0.));
#3773=DIRECTION('center_axis',(0.,0.,1.));
#3774=DIRECTION('ref_axis',(1.,0.,0.));
#3775=DIRECTION('axis',(0.,0.,1.));
#3776=DIRECTION('refdir',(1.,0.,0.));
#3777=DIRECTION('center_axis',(0.,0.,1.));
#3778=DIRECTION('ref_axis',(1.,0.,0.));
#3779=DIRECTION('center_axis',(0.,0.,-1.));
#3780=DIRECTION('ref_axis',(1.,0.,0.));
#3781=DIRECTION('',(0.,0.,-1.));
#3782=DIRECTION('center_axis',(0.,0.,-1.));
#3783=DIRECTION('ref_axis',(1.,0.,0.));
#3784=DIRECTION('center_axis',(0.,0.,1.));
#3785=DIRECTION('ref_axis',(1.,0.,0.));
#3786=DIRECTION('center_axis',(0.,0.,1.));
#3787=DIRECTION('ref_axis',(1.,0.,0.));
#3788=DIRECTION('',(0.,0.,-1.));
#3789=DIRECTION('center_axis',(0.,0.,1.));
#3790=DIRECTION('ref_axis',(1.,0.,0.));
#3791=DIRECTION('center_axis',(0.,0.,1.));
#3792=DIRECTION('ref_axis',(1.,0.,0.));
#3793=DIRECTION('center_axis',(0.,0.,1.));
#3794=DIRECTION('ref_axis',(1.,0.,0.));
#3795=DIRECTION('axis',(0.,0.,1.));
#3796=DIRECTION('refdir',(1.,0.,0.));
#3797=DIRECTION('center_axis',(-1.,0.,0.));
#3798=DIRECTION('ref_axis',(0.,1.,0.));
#3799=DIRECTION('',(0.,0.,1.));
#3800=DIRECTION('',(0.,-1.,0.));
#3801=DIRECTION('',(0.,0.,-1.));
#3802=DIRECTION('',(0.,1.,0.));
#3803=DIRECTION('center_axis',(1.,0.,0.));
#3804=DIRECTION('ref_axis',(0.,-1.,0.));
#3805=DIRECTION('',(0.,0.,-1.));
#3806=DIRECTION('',(0.,-1.,0.));
#3807=DIRECTION('',(0.,0.,1.));
#3808=DIRECTION('',(0.,1.,0.));
#3809=DIRECTION('center_axis',(0.,0.,1.));
#3810=DIRECTION('ref_axis',(1.,0.,0.));
#3811=DIRECTION('center_axis',(0.,0.,1.));
#3812=DIRECTION('ref_axis',(1.,0.,0.));
#3813=DIRECTION('center_axis',(0.,0.,-1.));
#3814=DIRECTION('ref_axis',(1.,0.,0.));
#3815=DIRECTION('center_axis',(0.,0.,1.));
#3816=DIRECTION('ref_axis',(6.12323399573677E-17,-1.,0.));
#3817=DIRECTION('center_axis',(0.,0.,-1.));
#3818=DIRECTION('ref_axis',(1.,0.,0.));
#3819=DIRECTION('center_axis',(0.,0.,1.));
#3820=DIRECTION('ref_axis',(6.12323399573677E-17,-1.,0.));
#3821=DIRECTION('center_axis',(0.,0.,1.));
#3822=DIRECTION('ref_axis',(1.,0.,0.));
#3823=DIRECTION('center_axis',(0.,0.,1.));
#3824=DIRECTION('ref_axis',(1.,0.,0.));
#3825=DIRECTION('',(0.,-1.,0.));
#3826=DIRECTION('',(1.,0.,0.));
#3827=DIRECTION('',(0.,-1.,0.));
#3828=DIRECTION('',(0.87035559565211,0.,-0.492423737361495));
#3829=DIRECTION('',(0.,-1.,0.));
#3830=DIRECTION('',(1.,0.,0.));
#3831=DIRECTION('',(0.,-1.,0.));
#3832=DIRECTION('',(1.,0.,0.));
#3833=DIRECTION('',(0.,-1.,0.));
#3834=DIRECTION('',(1.,0.,0.));
#3835=DIRECTION('',(0.,-1.,0.));
#3836=DIRECTION('',(1.,0.,0.));
#3837=DIRECTION('',(0.,-1.,0.));
#3838=DIRECTION('',(1.,0.,0.));
#3839=DIRECTION('',(0.,-1.,0.));
#3840=DIRECTION('',(0.87035559565211,0.,-0.492423737361495));
#3841=DIRECTION('',(0.,-1.,0.));
#3842=DIRECTION('',(1.,0.,0.));
#3843=DIRECTION('',(0.,-1.,0.));
#3844=DIRECTION('',(1.,0.,0.));
#3845=DIRECTION('',(0.,-1.,0.));
#3846=DIRECTION('',(1.,0.,0.));
#3847=DIRECTION('',(0.,-1.,0.));
#3848=DIRECTION('',(1.,0.,0.));
#3849=DIRECTION('',(0.,-1.,0.));
#3850=DIRECTION('',(1.,0.,0.));
#3851=DIRECTION('',(0.,-1.,0.));
#3852=DIRECTION('',(1.,0.,0.));
#3853=DIRECTION('',(0.,-1.,0.));
#3854=DIRECTION('',(0.314104961082827,0.,-0.949388262737199));
#3855=DIRECTION('',(0.,-1.,0.));
#3856=DIRECTION('',(1.,0.,0.));
#3857=DIRECTION('',(0.,-1.,0.));
#3858=DIRECTION('',(0.999985664762424,0.,0.0053544625925562));
#3859=DIRECTION('',(0.,-1.,0.));
#3860=DIRECTION('',(1.,0.,0.));
#3861=DIRECTION('',(0.,-1.,0.));
#3862=DIRECTION('',(1.,0.,0.));
#3863=DIRECTION('',(0.,-1.,0.));
#3864=DIRECTION('',(1.,0.,0.));
#3865=DIRECTION('',(0.,-1.,0.));
#3866=DIRECTION('',(1.,0.,0.));
#3867=CARTESIAN_POINT('',(0.,0.,0.));
#3868=CARTESIAN_POINT('',(0.,0.,0.));
#3869=CARTESIAN_POINT('Origin',(26.8635279142892,-43.8446218822583,5.));
#3870=CARTESIAN_POINT('',(22.8635279142892,-43.8446218822583,10.));
#3871=CARTESIAN_POINT('Origin',(26.8635279142892,-43.8446218822583,10.));
#3872=CARTESIAN_POINT('',(22.8635279142892,-43.8446218822583,0.));
#3873=CARTESIAN_POINT('',(22.8635279142892,-43.8446218822583,5.));
#3874=CARTESIAN_POINT('Origin',(26.8635279142892,-43.8446218822583,0.));
#3875=CARTESIAN_POINT('Origin',(0.,0.,5.));
#3876=CARTESIAN_POINT('',(-5.,6.12323399573677E-16,10.));
#3877=CARTESIAN_POINT('Origin',(0.,0.,10.));
#3878=CARTESIAN_POINT('',(-5.,6.12323399573677E-16,0.));
#3879=CARTESIAN_POINT('',(-5.,6.12323399573677E-16,5.));
#3880=CARTESIAN_POINT('Origin',(0.,0.,0.));
#3881=CARTESIAN_POINT('Origin',(55.,-95.,-35.));
#3882=CARTESIAN_POINT('',(55.,-105.,-30.5));
#3883=CARTESIAN_POINT('Origin',(55.,-105.,-35.));
#3884=CARTESIAN_POINT('',(55.,-90.,-30.5));
#3885=CARTESIAN_POINT('',(55.,-95.,-30.5));
#3886=CARTESIAN_POINT('Origin',(55.,-90.,-35.));
#3887=CARTESIAN_POINT('Origin',(-55.,-95.,-35.));
#3888=CARTESIAN_POINT('',(-55.,-105.,-30.5));
#3889=CARTESIAN_POINT('Origin',(-55.,-105.,-35.));
#3890=CARTESIAN_POINT('',(-55.,-90.,-30.5));
#3891=CARTESIAN_POINT('',(-55.,-95.,-30.5));
#3892=CARTESIAN_POINT('Origin',(-55.,-90.,-35.));
#3893=CARTESIAN_POINT('Origin',(-55.,-95.,35.));
#3894=CARTESIAN_POINT('',(-55.,-105.,39.5));
#3895=CARTESIAN_POINT('Origin',(-55.,-105.,35.));
#3896=CARTESIAN_POINT('',(-55.,-90.,39.5));
#3897=CARTESIAN_POINT('',(-55.,-95.,39.5));
#3898=CARTESIAN_POINT('Origin',(-55.,-90.,35.));
#3899=CARTESIAN_POINT('Origin',(55.,-95.,35.));
#3900=CARTESIAN_POINT('',(55.,-105.,39.5));
#3901=CARTESIAN_POINT('Origin',(55.,-105.,35.));
#3902=CARTESIAN_POINT('',(55.,-90.,39.5));
#3903=CARTESIAN_POINT('',(55.,-95.,39.5));
#3904=CARTESIAN_POINT('Origin',(55.,-90.,35.));
#3905=CARTESIAN_POINT('Origin',(70.,-90.,-40.));
#3906=CARTESIAN_POINT('',(-70.,-90.,0.));
#3907=CARTESIAN_POINT('',(70.,-90.,0.));
#3908=CARTESIAN_POINT('',(-70.,-90.,0.));
#3909=CARTESIAN_POINT('',(70.,-90.,-60.));
#3910=CARTESIAN_POINT('',(70.,-90.,-40.));
#3911=CARTESIAN_POINT('',(-70.,-90.,-60.));
#3912=CARTESIAN_POINT('',(35.,-90.,-60.));
#3913=CARTESIAN_POINT('',(-70.,-90.,-40.));
#3914=CARTESIAN_POINT('Origin',(70.,-90.,-40.));
#3915=CARTESIAN_POINT('',(-70.,-90.,10.));
#3916=CARTESIAN_POINT('',(70.,-90.,10.));
#3917=CARTESIAN_POINT('',(-70.,-90.,10.));
#3918=CARTESIAN_POINT('',(-70.,-90.,60.));
#3919=CARTESIAN_POINT('',(-70.,-90.,-40.));
#3920=CARTESIAN_POINT('',(70.,-90.,60.));
#3921=CARTESIAN_POINT('',(70.,-90.,60.));
#3922=CARTESIAN_POINT('',(70.,-90.,-40.));
#3923=CARTESIAN_POINT('Origin',(-70.,-105.,-40.));
#3924=CARTESIAN_POINT('',(-70.,-105.,-60.));
#3925=CARTESIAN_POINT('',(70.,-105.,-60.));
#3926=CARTESIAN_POINT('',(-35.,-105.,-60.));
#3927=CARTESIAN_POINT('',(70.,-105.,60.));
#3928=CARTESIAN_POINT('',(70.,-105.,-20.));
#3929=CARTESIAN_POINT('',(-70.,-105.,60.));
#3930=CARTESIAN_POINT('',(-35.,-105.,60.));
#3931=CARTESIAN_POINT('',(-70.,-105.,-20.));
#3932=CARTESIAN_POINT('Origin',(0.,-95.,60.));
#3933=CARTESIAN_POINT('',(-70.,-90.,60.));
#3934=CARTESIAN_POINT('',(70.,-100.,60.));
#3935=CARTESIAN_POINT('Origin',(0.,-95.,-60.));
#3936=CARTESIAN_POINT('',(-70.,-2.5,-60.));
#3937=CARTESIAN_POINT('',(70.,-92.5,-60.));
#3938=CARTESIAN_POINT('Origin',(70.,80.,0.));
#3939=CARTESIAN_POINT('',(70.,80.,0.));
#3940=CARTESIAN_POINT('',(-70.,80.,0.));
#3941=CARTESIAN_POINT('',(35.,80.,0.));
#3942=CARTESIAN_POINT('',(-70.,80.,10.));
#3943=CARTESIAN_POINT('',(-70.,80.,0.));
#3944=CARTESIAN_POINT('',(70.,80.,10.));
#3945=CARTESIAN_POINT('',(35.,80.,10.));
#3946=CARTESIAN_POINT('',(70.,80.,0.));
#3947=CARTESIAN_POINT('Origin',(70.,-90.,0.));
#3948=CARTESIAN_POINT('',(70.,-90.,0.));
#3949=CARTESIAN_POINT('',(70.,-90.,10.));
#3950=CARTESIAN_POINT('Origin',(-70.,90.,0.));
#3951=CARTESIAN_POINT('',(-70.,90.,0.));
#3952=CARTESIAN_POINT('',(-70.,90.,10.));
#3953=CARTESIAN_POINT('Origin',(0.,0.,10.));
#3954=CARTESIAN_POINT('Origin',(0.,0.,0.));
#3955=CARTESIAN_POINT('',(0.,0.,0.));
#3956=CARTESIAN_POINT('Origin',(0.,0.,4.));
#3957=CARTESIAN_POINT('',(-6.,7.34788079488412E-16,8.));
#3958=CARTESIAN_POINT('Origin',(0.,0.,8.));
#3959=CARTESIAN_POINT('',(-6.,7.34788079488412E-16,0.));
#3960=CARTESIAN_POINT('',(-6.,7.34788079488412E-16,4.));
#3961=CARTESIAN_POINT('Origin',(0.,0.,0.));
#3962=CARTESIAN_POINT('Origin',(30.4338085214449,-9.88854381999833,0.));
#3963=CARTESIAN_POINT('',(30.4338085214449,-9.88854381999833,0.));
#3964=CARTESIAN_POINT('',(38.0422606518061,-12.3606797749979,0.));
#3965=CARTESIAN_POINT('',(30.4338085214449,-9.88854381999833,0.));
#3966=CARTESIAN_POINT('',(38.0422606518061,-12.3606797749979,8.));
#3967=CARTESIAN_POINT('',(38.0422606518061,-12.3606797749979,0.));
#3968=CARTESIAN_POINT('',(30.4338085214449,-9.88854381999833,8.));
#3969=CARTESIAN_POINT('',(30.4338085214449,-9.88854381999833,8.));
#3970=CARTESIAN_POINT('',(30.4338085214449,-9.88854381999833,0.));
#3971=CARTESIAN_POINT('Origin',(32.3606797749979,-23.5114100916989,0.));
#3972=CARTESIAN_POINT('',(32.3606797749979,-23.5114100916989,0.));
#3973=CARTESIAN_POINT('',(32.3606797749979,-23.5114100916989,0.));
#3974=CARTESIAN_POINT('',(32.3606797749979,-23.5114100916989,8.));
#3975=CARTESIAN_POINT('',(32.3606797749979,-23.5114100916989,8.));
#3976=CARTESIAN_POINT('',(32.3606797749979,-23.5114100916989,0.));
#3977=CARTESIAN_POINT('Origin',(25.8885438199983,-18.8091280733591,0.));
#3978=CARTESIAN_POINT('',(25.8885438199983,-18.8091280733591,0.));
#3979=CARTESIAN_POINT('',(25.8885438199983,-18.8091280733591,0.));
#3980=CARTESIAN_POINT('',(25.8885438199983,-18.8091280733591,8.));
#3981=CARTESIAN_POINT('',(25.8885438199983,-18.8091280733591,8.));
#3982=CARTESIAN_POINT('',(25.8885438199983,-18.8091280733591,0.));
#3983=CARTESIAN_POINT('Origin',(23.5114100916989,-32.3606797749979,0.));
#3984=CARTESIAN_POINT('',(23.5114100916989,-32.3606797749979,0.));
#3985=CARTESIAN_POINT('',(23.5114100916989,-32.3606797749979,0.));
#3986=CARTESIAN_POINT('',(23.5114100916989,-32.3606797749979,8.));
#3987=CARTESIAN_POINT('',(23.5114100916989,-32.3606797749979,8.));
#3988=CARTESIAN_POINT('',(23.5114100916989,-32.3606797749979,0.));
#3989=CARTESIAN_POINT('Origin',(18.8091280733591,-25.8885438199983,0.));
#3990=CARTESIAN_POINT('',(18.8091280733591,-25.8885438199983,0.));
#3991=CARTESIAN_POINT('',(18.8091280733591,-25.8885438199983,0.));
#3992=CARTESIAN_POINT('',(18.8091280733591,-25.8885438199983,8.));
#3993=CARTESIAN_POINT('',(18.8091280733591,-25.8885438199983,8.));
#3994=CARTESIAN_POINT('',(18.8091280733591,-25.8885438199983,0.));
#3995=CARTESIAN_POINT('Origin',(12.3606797749979,-38.0422606518061,0.));
#3996=CARTESIAN_POINT('',(12.3606797749979,-38.0422606518061,0.));
#3997=CARTESIAN_POINT('',(12.3606797749979,-38.0422606518061,0.));
#3998=CARTESIAN_POINT('',(12.3606797749979,-38.0422606518061,8.));
#3999=CARTESIAN_POINT('',(12.3606797749979,-38.0422606518061,8.));
#4000=CARTESIAN_POINT('',(12.3606797749979,-38.0422606518061,0.));
#4001=CARTESIAN_POINT('Origin',(9.88854381999831,-30.4338085214449,0.));
#4002=CARTESIAN_POINT('',(9.88854381999831,-30.4338085214449,0.));
#4003=CARTESIAN_POINT('',(9.88854381999831,-30.4338085214449,0.));
#4004=CARTESIAN_POINT('',(9.88854381999831,-30.4338085214449,8.));
#4005=CARTESIAN_POINT('',(9.88854381999831,-30.4338085214449,8.));
#4006=CARTESIAN_POINT('',(9.88854381999831,-30.4338085214449,0.));
#4007=CARTESIAN_POINT('Origin',(-7.34788079488412E-15,-40.,0.));
#4008=CARTESIAN_POINT('',(-7.34788079488412E-15,-40.,0.));
#4009=CARTESIAN_POINT('',(-7.34788079488412E-15,-40.,0.));
#4010=CARTESIAN_POINT('',(-8.88178419700125E-15,-40.,8.));
#4011=CARTESIAN_POINT('',(-7.34788079488412E-15,-40.,8.));
#4012=CARTESIAN_POINT('',(-7.34788079488412E-15,-40.,0.));
#4013=CARTESIAN_POINT('Origin',(-5.8783046359073E-15,-32.,0.));
#4014=CARTESIAN_POINT('',(-5.8783046359073E-15,-32.,0.));
#4015=CARTESIAN_POINT('',(-5.8783046359073E-15,-32.,0.));
#4016=CARTESIAN_POINT('',(-4.44089209850063E-15,-32.,8.));
#4017=CARTESIAN_POINT('',(-5.8783046359073E-15,-32.,8.));
#4018=CARTESIAN_POINT('',(-5.8783046359073E-15,-32.,0.));
#4019=CARTESIAN_POINT('Origin',(-12.3606797749979,-38.0422606518061,0.));
#4020=CARTESIAN_POINT('',(-12.3606797749979,-38.0422606518061,0.));
#4021=CARTESIAN_POINT('',(-12.3606797749979,-38.0422606518061,0.));
#4022=CARTESIAN_POINT('',(-12.3606797749979,-38.0422606518061,8.));
#4023=CARTESIAN_POINT('',(-12.3606797749979,-38.0422606518061,8.));
#4024=CARTESIAN_POINT('',(-12.3606797749979,-38.0422606518061,0.));
#4025=CARTESIAN_POINT('Origin',(-9.88854381999832,-30.4338085214449,0.));
#4026=CARTESIAN_POINT('',(-9.88854381999832,-30.4338085214449,0.));
#4027=CARTESIAN_POINT('',(-9.88854381999832,-30.4338085214449,0.));
#4028=CARTESIAN_POINT('',(-9.88854381999833,-30.4338085214449,8.));
#4029=CARTESIAN_POINT('',(-9.88854381999832,-30.4338085214449,8.));
#4030=CARTESIAN_POINT('',(-9.88854381999832,-30.4338085214449,0.));
#4031=CARTESIAN_POINT('Origin',(-23.5114100916989,-32.3606797749979,0.));
#4032=CARTESIAN_POINT('',(-23.5114100916989,-32.3606797749979,0.));
#4033=CARTESIAN_POINT('',(-23.5114100916989,-32.3606797749979,0.));
#4034=CARTESIAN_POINT('',(-23.5114100916989,-32.3606797749979,8.));
#4035=CARTESIAN_POINT('',(-23.5114100916989,-32.3606797749979,8.));
#4036=CARTESIAN_POINT('',(-23.5114100916989,-32.3606797749979,0.));
#4037=CARTESIAN_POINT('Origin',(-18.8091280733591,-25.8885438199983,0.));
#4038=CARTESIAN_POINT('',(-18.8091280733591,-25.8885438199983,0.));
#4039=CARTESIAN_POINT('',(-18.8091280733591,-25.8885438199983,0.));
#4040=CARTESIAN_POINT('',(-18.8091280733591,-25.8885438199983,8.));
#4041=CARTESIAN_POINT('',(-18.8091280733591,-25.8885438199983,8.));
#4042=CARTESIAN_POINT('',(-18.8091280733591,-25.8885438199983,0.));
#4043=CARTESIAN_POINT('Origin',(-32.3606797749979,-23.5114100916989,0.));
#4044=CARTESIAN_POINT('',(-32.3606797749979,-23.5114100916989,0.));
#4045=CARTESIAN_POINT('',(-32.3606797749979,-23.5114100916989,0.));
#4046=CARTESIAN_POINT('',(-32.3606797749979,-23.5114100916989,8.));
#4047=CARTESIAN_POINT('',(-32.3606797749979,-23.5114100916989,8.));
#4048=CARTESIAN_POINT('',(-32.3606797749979,-23.5114100916989,0.));
#4049=CARTESIAN_POINT('Origin',(-25.8885438199983,-18.8091280733591,0.));
#4050=CARTESIAN_POINT('',(-25.8885438199983,-18.8091280733591,0.));
#4051=CARTESIAN_POINT('',(-25.8885438199983,-18.8091280733591,0.));
#4052=CARTESIAN_POINT('',(-25.8885438199983,-18.8091280733591,8.));
#4053=CARTESIAN_POINT('',(-25.8885438199983,-18.8091280733591,8.));
#4054=CARTESIAN_POINT('',(-25.8885438199983,-18.8091280733591,0.));
#4055=CARTESIAN_POINT('Origin',(-38.0422606518061,-12.3606797749979,0.));
#4056=CARTESIAN_POINT('',(-38.0422606518061,-12.3606797749979,0.));
#4057=CARTESIAN_POINT('',(-38.0422606518061,-12.3606797749979,0.));
#4058=CARTESIAN_POINT('',(-38.0422606518061,-12.3606797749979,8.));
#4059=CARTESIAN_POINT('',(-38.0422606518061,-12.3606797749979,8.));
#4060=CARTESIAN_POINT('',(-38.0422606518061,-12.3606797749979,0.));
#4061=CARTESIAN_POINT('Origin',(-30.4338085214449,-9.88854381999831,0.));
#4062=CARTESIAN_POINT('',(-30.4338085214449,-9.88854381999831,0.));
#4063=CARTESIAN_POINT('',(-30.4338085214449,-9.88854381999831,0.));
#4064=CARTESIAN_POINT('',(-30.4338085214449,-9.88854381999831,8.));
#4065=CARTESIAN_POINT('',(-30.4338085214449,-9.88854381999831,8.));
#4066=CARTESIAN_POINT('',(-30.4338085214449,-9.88854381999831,0.));
#4067=CARTESIAN_POINT('Origin',(-40.,4.89858719658941E-15,0.));
#4068=CARTESIAN_POINT('',(-40.,4.89858719658941E-15,0.));
#4069=CARTESIAN_POINT('',(-40.,4.89858719658941E-15,0.));
#4070=CARTESIAN_POINT('',(-40.,4.44089209850063E-15,8.));
#4071=CARTESIAN_POINT('',(-40.,4.89858719658941E-15,8.));
#4072=CARTESIAN_POINT('',(-40.,4.89858719658941E-15,0.));
#4073=CARTESIAN_POINT('Origin',(-32.,3.91886975727153E-15,0.));
#4074=CARTESIAN_POINT('',(-32.,3.91886975727153E-15,0.));
#4075=CARTESIAN_POINT('',(-32.,3.91886975727153E-15,0.));
#4076=CARTESIAN_POINT('',(-32.,4.44089209850063E-15,8.));
#4077=CARTESIAN_POINT('',(-32.,3.91886975727153E-15,8.));
#4078=CARTESIAN_POINT('',(-32.,3.91886975727153E-15,0.));
#4079=CARTESIAN_POINT('Origin',(-38.0422606518061,12.3606797749979,0.));
#4080=CARTESIAN_POINT('',(-38.0422606518061,12.3606797749979,0.));
#4081=CARTESIAN_POINT('',(-38.0422606518061,12.3606797749979,0.));
#4082=CARTESIAN_POINT('',(-38.0422606518061,12.3606797749979,8.));
#4083=CARTESIAN_POINT('',(-38.0422606518061,12.3606797749979,8.));
#4084=CARTESIAN_POINT('',(-38.0422606518061,12.3606797749979,0.));
#4085=CARTESIAN_POINT('Origin',(-30.4338085214449,9.88854381999832,0.));
#4086=CARTESIAN_POINT('',(-30.4338085214449,9.88854381999832,0.));
#4087=CARTESIAN_POINT('',(-30.4338085214449,9.88854381999832,0.));
#4088=CARTESIAN_POINT('',(-30.4338085214449,9.88854381999832,8.));
#4089=CARTESIAN_POINT('',(-30.4338085214449,9.88854381999832,8.));
#4090=CARTESIAN_POINT('',(-30.4338085214449,9.88854381999832,0.));
#4091=CARTESIAN_POINT('Origin',(-32.3606797749979,23.5114100916989,0.));
#4092=CARTESIAN_POINT('',(-32.3606797749979,23.5114100916989,0.));
#4093=CARTESIAN_POINT('',(-32.3606797749979,23.5114100916989,0.));
#4094=CARTESIAN_POINT('',(-32.3606797749979,23.5114100916989,8.));
#4095=CARTESIAN_POINT('',(-32.3606797749979,23.5114100916989,8.));
#4096=CARTESIAN_POINT('',(-32.3606797749979,23.5114100916989,0.));
#4097=CARTESIAN_POINT('Origin',(-25.8885438199983,18.8091280733591,0.));
#4098=CARTESIAN_POINT('',(-25.8885438199983,18.8091280733591,0.));
#4099=CARTESIAN_POINT('',(-25.8885438199983,18.8091280733591,0.));
#4100=CARTESIAN_POINT('',(-25.8885438199983,18.8091280733591,8.));
#4101=CARTESIAN_POINT('',(-25.8885438199983,18.8091280733591,8.));
#4102=CARTESIAN_POINT('',(-25.8885438199983,18.8091280733591,0.));
#4103=CARTESIAN_POINT('Origin',(-23.5114100916989,32.3606797749979,0.));
#4104=CARTESIAN_POINT('',(-23.5114100916989,32.3606797749979,0.));
#4105=CARTESIAN_POINT('',(-23.5114100916989,32.3606797749979,0.));
#4106=CARTESIAN_POINT('',(-23.5114100916989,32.3606797749979,8.));
#4107=CARTESIAN_POINT('',(-23.5114100916989,32.3606797749979,8.));
#4108=CARTESIAN_POINT('',(-23.5114100916989,32.3606797749979,0.));
#4109=CARTESIAN_POINT('Origin',(-18.8091280733591,25.8885438199983,0.));
#4110=CARTESIAN_POINT('',(-18.8091280733591,25.8885438199983,0.));
#4111=CARTESIAN_POINT('',(-18.8091280733591,25.8885438199983,0.));
#4112=CARTESIAN_POINT('',(-18.8091280733591,25.8885438199983,8.));
#4113=CARTESIAN_POINT('',(-18.8091280733591,25.8885438199983,8.));
#4114=CARTESIAN_POINT('',(-18.8091280733591,25.8885438199983,0.));
#4115=CARTESIAN_POINT('Origin',(-12.3606797749979,38.0422606518061,0.));
#4116=CARTESIAN_POINT('',(-12.3606797749979,38.0422606518061,0.));
#4117=CARTESIAN_POINT('',(-12.3606797749979,38.0422606518061,0.));
#4118=CARTESIAN_POINT('',(-12.3606797749979,38.0422606518061,8.));
#4119=CARTESIAN_POINT('',(-12.3606797749979,38.0422606518061,8.));
#4120=CARTESIAN_POINT('',(-12.3606797749979,38.0422606518061,0.));
#4121=CARTESIAN_POINT('Origin',(-9.88854381999831,30.4338085214449,0.));
#4122=CARTESIAN_POINT('',(-9.88854381999831,30.4338085214449,0.));
#4123=CARTESIAN_POINT('',(-9.88854381999831,30.4338085214449,0.));
#4124=CARTESIAN_POINT('',(-9.88854381999832,30.4338085214449,8.));
#4125=CARTESIAN_POINT('',(-9.88854381999831,30.4338085214449,8.));
#4126=CARTESIAN_POINT('',(-9.88854381999831,30.4338085214449,0.));
#4127=CARTESIAN_POINT('Origin',(2.44929359829471E-15,40.,0.));
#4128=CARTESIAN_POINT('',(2.44929359829471E-15,40.,0.));
#4129=CARTESIAN_POINT('',(2.44929359829471E-15,40.,0.));
#4130=CARTESIAN_POINT('',(4.44089209850063E-15,40.,8.));
#4131=CARTESIAN_POINT('',(2.44929359829471E-15,40.,8.));
#4132=CARTESIAN_POINT('',(2.44929359829471E-15,40.,0.));
#4133=CARTESIAN_POINT('Origin',(1.95943487863577E-15,32.,0.));
#4134=CARTESIAN_POINT('',(1.95943487863577E-15,32.,0.));
#4135=CARTESIAN_POINT('',(1.95943487863577E-15,32.,0.));
#4136=CARTESIAN_POINT('',(0.,32.,8.));
#4137=CARTESIAN_POINT('',(1.95943487863577E-15,32.,8.));
#4138=CARTESIAN_POINT('',(1.95943487863577E-15,32.,0.));
#4139=CARTESIAN_POINT('Origin',(12.3606797749979,38.0422606518061,0.));
#4140=CARTESIAN_POINT('',(12.3606797749979,38.0422606518061,0.));
#4141=CARTESIAN_POINT('',(12.3606797749979,38.0422606518061,0.));
#4142=CARTESIAN_POINT('',(12.3606797749979,38.0422606518061,8.));
#4143=CARTESIAN_POINT('',(12.3606797749979,38.0422606518061,8.));
#4144=CARTESIAN_POINT('',(12.3606797749979,38.0422606518061,0.));
#4145=CARTESIAN_POINT('Origin',(9.88854381999832,30.4338085214449,0.));
#4146=CARTESIAN_POINT('',(9.88854381999832,30.4338085214449,0.));
#4147=CARTESIAN_POINT('',(9.88854381999832,30.4338085214449,0.));
#4148=CARTESIAN_POINT('',(9.88854381999832,30.4338085214449,8.));
#4149=CARTESIAN_POINT('',(9.88854381999832,30.4338085214449,8.));
#4150=CARTESIAN_POINT('',(9.88854381999832,30.4338085214449,0.));
#4151=CARTESIAN_POINT('Origin',(23.5114100916989,32.3606797749979,0.));
#4152=CARTESIAN_POINT('',(23.5114100916989,32.3606797749979,0.));
#4153=CARTESIAN_POINT('',(23.5114100916989,32.3606797749979,0.));
#4154=CARTESIAN_POINT('',(23.5114100916989,32.3606797749979,8.));
#4155=CARTESIAN_POINT('',(23.5114100916989,32.3606797749979,8.));
#4156=CARTESIAN_POINT('',(23.5114100916989,32.3606797749979,0.));
#4157=CARTESIAN_POINT('Origin',(18.8091280733591,25.8885438199983,0.));
#4158=CARTESIAN_POINT('',(18.8091280733591,25.8885438199983,0.));
#4159=CARTESIAN_POINT('',(18.8091280733591,25.8885438199983,0.));
#4160=CARTESIAN_POINT('',(18.8091280733591,25.8885438199983,8.));
#4161=CARTESIAN_POINT('',(18.8091280733591,25.8885438199983,8.));
#4162=CARTESIAN_POINT('',(18.8091280733591,25.8885438199983,0.));
#4163=CARTESIAN_POINT('Origin',(32.3606797749979,23.5114100916989,0.));
#4164=CARTESIAN_POINT('',(32.3606797749979,23.5114100916989,0.));
#4165=CARTESIAN_POINT('',(32.3606797749979,23.5114100916989,0.));
#4166=CARTESIAN_POINT('',(32.3606797749979,23.5114100916989,8.));
#4167=CARTESIAN_POINT('',(32.3606797749979,23.5114100916989,8.));
#4168=CARTESIAN_POINT('',(32.3606797749979,23.5114100916989,0.));
#4169=CARTESIAN_POINT('Origin',(25.8885438199983,18.8091280733591,0.));
#4170=CARTESIAN_POINT('',(25.8885438199983,18.8091280733591,0.));
#4171=CARTESIAN_POINT('',(25.8885438199983,18.8091280733591,0.));
#4172=CARTESIAN_POINT('',(25.8885438199983,18.8091280733591,8.));
#4173=CARTESIAN_POINT('',(25.8885438199983,18.8091280733591,8.));
#4174=CARTESIAN_POINT('',(25.8885438199983,18.8091280733591,0.));
#4175=CARTESIAN_POINT('Origin',(38.0422606518061,12.3606797749979,0.));
#4176=CARTESIAN_POINT('',(38.0422606518061,12.3606797749979,0.));
#4177=CARTESIAN_POINT('',(38.0422606518061,12.3606797749979,0.));
#4178=CARTESIAN_POINT('',(38.0422606518061,12.3606797749979,8.));
#4179=CARTESIAN_POINT('',(38.0422606518061,12.3606797749979,8.));
#4180=CARTESIAN_POINT('',(38.0422606518061,12.3606797749979,0.));
#4181=CARTESIAN_POINT('Origin',(30.4338085214449,9.88854381999832,0.));
#4182=CARTESIAN_POINT('',(30.4338085214449,9.88854381999832,0.));
#4183=CARTESIAN_POINT('',(30.4338085214449,9.88854381999832,0.));
#4184=CARTESIAN_POINT('',(30.4338085214449,9.88854381999832,8.));
#4185=CARTESIAN_POINT('',(30.4338085214449,9.88854381999832,8.));
#4186=CARTESIAN_POINT('',(30.4338085214449,9.88854381999832,0.));
#4187=CARTESIAN_POINT('Origin',(40.,0.,0.));
#4188=CARTESIAN_POINT('',(40.,0.,0.));
#4189=CARTESIAN_POINT('',(40.,0.,0.));
#4190=CARTESIAN_POINT('',(40.,0.,8.));
#4191=CARTESIAN_POINT('',(40.,0.,8.));
#4192=CARTESIAN_POINT('',(40.,0.,0.));
#4193=CARTESIAN_POINT('Origin',(32.,0.,0.));
#4194=CARTESIAN_POINT('',(32.,0.,0.));
#4195=CARTESIAN_POINT('',(32.,0.,0.));
#4196=CARTESIAN_POINT('',(32.,0.,8.));
#4197=CARTESIAN_POINT('',(32.,0.,8.));
#4198=CARTESIAN_POINT('',(32.,0.,0.));
#4199=CARTESIAN_POINT('Origin',(38.0422606518061,-12.3606797749979,0.));
#4200=CARTESIAN_POINT('',(38.0422606518061,-12.3606797749979,0.));
#4201=CARTESIAN_POINT('',(38.0422606518061,-12.3606797749979,8.));
#4202=CARTESIAN_POINT('Origin',(0.,0.,8.));
#4203=CARTESIAN_POINT('Origin',(0.,0.,0.));
#4204=CARTESIAN_POINT('',(0.,0.,0.));
#4205=CARTESIAN_POINT('Origin',(85.,0.,4.));
#4206=CARTESIAN_POINT('',(78.,8.57252759403147E-16,8.));
#4207=CARTESIAN_POINT('Origin',(85.,0.,8.));
#4208=CARTESIAN_POINT('',(78.,8.57252759403147E-16,0.));
#4209=CARTESIAN_POINT('',(78.,8.57252759403147E-16,4.));
#4210=CARTESIAN_POINT('Origin',(85.,0.,0.));
#4211=CARTESIAN_POINT('Origin',(50.,12.,4.));
#4212=CARTESIAN_POINT('',(46.,12.,8.));
#4213=CARTESIAN_POINT('Origin',(50.,12.,8.));
#4214=CARTESIAN_POINT('',(46.,12.,0.));
#4215=CARTESIAN_POINT('',(46.,12.,4.));
#4216=CARTESIAN_POINT('Origin',(50.,12.,0.));
#4217=CARTESIAN_POINT('Origin',(0.,0.,4.));
#4218=CARTESIAN_POINT('',(-6.,7.34788079488412E-16,8.));
#4219=CARTESIAN_POINT('Origin',(0.,0.,8.));
#4220=CARTESIAN_POINT('',(-6.,7.34788079488412E-16,0.));
#4221=CARTESIAN_POINT('',(-6.,7.34788079488412E-16,4.));
#4222=CARTESIAN_POINT('Origin',(0.,0.,0.));
#4223=CARTESIAN_POINT('Origin',(-20.,15.,0.));
#4224=CARTESIAN_POINT('',(-20.,15.,0.));
#4225=CARTESIAN_POINT('',(-20.,-15.,0.));
#4226=CARTESIAN_POINT('',(-20.,15.,0.));
#4227=CARTESIAN_POINT('',(-20.,-15.,8.));
#4228=CARTESIAN_POINT('',(-20.,-15.,0.));
#4229=CARTESIAN_POINT('',(-20.,15.,8.));
#4230=CARTESIAN_POINT('',(-20.,15.,8.));
#4231=CARTESIAN_POINT('',(-20.,15.,0.));
#4232=CARTESIAN_POINT('Origin',(-15.,20.,0.));
#4233=CARTESIAN_POINT('',(-15.,20.,0.));
#4234=CARTESIAN_POINT('',(-15.,20.,0.));
#4235=CARTESIAN_POINT('',(-15.,20.,8.));
#4236=CARTESIAN_POINT('',(-15.,20.,8.));
#4237=CARTESIAN_POINT('',(-15.,20.,0.));
#4238=CARTESIAN_POINT('Origin',(90.,20.,0.));
#4239=CARTESIAN_POINT('',(90.,20.,0.));
#4240=CARTESIAN_POINT('',(90.,20.,0.));
#4241=CARTESIAN_POINT('',(90.,20.,8.));
#4242=CARTESIAN_POINT('',(90.,20.,8.));
#4243=CARTESIAN_POINT('',(90.,20.,0.));
#4244=CARTESIAN_POINT('Origin',(100.,10.,0.));
#4245=CARTESIAN_POINT('',(100.,10.,0.));
#4246=CARTESIAN_POINT('',(100.,10.,0.));
#4247=CARTESIAN_POINT('',(100.,10.,8.));
#4248=CARTESIAN_POINT('',(100.,10.,8.));
#4249=CARTESIAN_POINT('',(100.,10.,0.));
#4250=CARTESIAN_POINT('Origin',(100.,-10.,0.));
#4251=CARTESIAN_POINT('',(100.,-10.,0.));
#4252=CARTESIAN_POINT('',(100.,-10.,0.));
#4253=CARTESIAN_POINT('',(100.,-10.,8.));
#4254=CARTESIAN_POINT('',(100.,-10.,8.));
#4255=CARTESIAN_POINT('',(100.,-10.,0.));
#4256=CARTESIAN_POINT('Origin',(90.,-20.,0.));
#4257=CARTESIAN_POINT('',(90.,-20.,0.));
#4258=CARTESIAN_POINT('',(90.,-20.,0.));
#4259=CARTESIAN_POINT('',(90.,-20.,8.));
#4260=CARTESIAN_POINT('',(90.,-20.,8.));
#4261=CARTESIAN_POINT('',(90.,-20.,0.));
#4262=CARTESIAN_POINT('Origin',(-15.,-20.,0.));
#4263=CARTESIAN_POINT('',(-15.,-20.,0.));
#4264=CARTESIAN_POINT('',(-15.,-20.,0.));
#4265=CARTESIAN_POINT('',(-15.,-20.,8.));
#4266=CARTESIAN_POINT('',(-15.,-20.,8.));
#4267=CARTESIAN_POINT('',(-15.,-20.,0.));
#4268=CARTESIAN_POINT('Origin',(-20.,-15.,0.));
#4269=CARTESIAN_POINT('',(-20.,-15.,0.));
#4270=CARTESIAN_POINT('',(-20.,-15.,8.));
#4271=CARTESIAN_POINT('Origin',(40.,0.,8.));
#4272=CARTESIAN_POINT('Origin',(40.,0.,0.));
#4273=CARTESIAN_POINT('',(0.,0.,0.));
#4274=CARTESIAN_POINT('Origin',(0.,0.,30.5));
#4275=CARTESIAN_POINT('',(-4.,-4.89858719658941E-16,30.));
#4276=CARTESIAN_POINT('Origin',(0.,0.,30.));
#4277=CARTESIAN_POINT('',(-4.,-4.89858719658941E-16,31.));
#4278=CARTESIAN_POINT('',(-4.,-4.89858719658941E-16,30.5));
#4279=CARTESIAN_POINT('Origin',(0.,0.,31.));
#4280=CARTESIAN_POINT('Origin',(8.,0.,30.));
#4281=CARTESIAN_POINT('',(-5.,6.12323399573677E-16,30.));
#4282=CARTESIAN_POINT('Origin',(0.,0.,30.));
#4283=CARTESIAN_POINT('Origin',(4.,0.,31.));
#4284=CARTESIAN_POINT('',(-5.,-6.12323399573677E-16,31.));
#4285=CARTESIAN_POINT('Origin',(0.,0.,31.));
#4286=CARTESIAN_POINT('Origin',(0.,0.,0.));
#4287=CARTESIAN_POINT('',(-5.,-6.12323399573677E-16,32.));
#4288=CARTESIAN_POINT('Origin',(0.,0.,32.));
#4289=CARTESIAN_POINT('',(-5.,-6.12323399573677E-16,0.));
#4290=CARTESIAN_POINT('Origin',(0.,0.,0.));
#4291=CARTESIAN_POINT('',(-8.,-9.79717439317883E-16,0.));
#4292=CARTESIAN_POINT('Origin',(0.,0.,0.));
#4293=CARTESIAN_POINT('',(-5.,-6.12323399573677E-16,0.));
#4294=CARTESIAN_POINT('Origin',(0.,0.,0.));
#4295=CARTESIAN_POINT('Origin',(0.,0.,-3.));
#4296=CARTESIAN_POINT('',(-8.,-9.79717439317883E-16,-3.));
#4297=CARTESIAN_POINT('',(-8.,-9.79717439317883E-16,-3.));
#4298=CARTESIAN_POINT('Origin',(0.,0.,-3.));
#4299=CARTESIAN_POINT('Origin',(0.,0.,-3.));
#4300=CARTESIAN_POINT('Origin',(0.,0.,0.));
#4301=CARTESIAN_POINT('',(-5.,-6.12323399573677E-16,0.));
#4302=CARTESIAN_POINT('Origin',(0.,0.,32.));
#4303=CARTESIAN_POINT('',(0.,0.,0.));
#4304=CARTESIAN_POINT('Origin',(0.,0.,18.5));
#4305=CARTESIAN_POINT('',(-3.,-3.67394039744206E-16,18.));
#4306=CARTESIAN_POINT('Origin',(0.,0.,18.));
#4307=CARTESIAN_POINT('',(-3.,-3.67394039744206E-16,19.));
#4308=CARTESIAN_POINT('',(-3.,-3.67394039744206E-16,18.5));
#4309=CARTESIAN_POINT('Origin',(0.,0.,19.));
#4310=CARTESIAN_POINT('Origin',(7.,0.,18.));
#4311=CARTESIAN_POINT('',(-4.,4.89858719658941E-16,18.));
#4312=CARTESIAN_POINT('Origin',(0.,0.,18.));
#4313=CARTESIAN_POINT('Origin',(3.,0.,19.));
#4314=CARTESIAN_POINT('',(-4.,-4.89858719658941E-16,19.));
#4315=CARTESIAN_POINT('Origin',(0.,0.,19.));
#4316=CARTESIAN_POINT('Origin',(0.,0.,0.));
#4317=CARTESIAN_POINT('',(-4.,-4.89858719658941E-16,20.));
#4318=CARTESIAN_POINT('Origin',(0.,0.,20.));
#4319=CARTESIAN_POINT('',(-4.,-4.89858719658941E-16,0.));
#4320=CARTESIAN_POINT('Origin',(0.,0.,0.));
#4321=CARTESIAN_POINT('',(-6.,-7.34788079488412E-16,0.));
#4322=CARTESIAN_POINT('Origin',(0.,0.,0.));
#4323=CARTESIAN_POINT('',(-4.,-4.89858719658941E-16,0.));
#4324=CARTESIAN_POINT('Origin',(0.,0.,0.));
#4325=CARTESIAN_POINT('Origin',(0.,0.,-2.));
#4326=CARTESIAN_POINT('',(-6.,-7.34788079488412E-16,-2.));
#4327=CARTESIAN_POINT('',(-6.,-7.34788079488412E-16,-2.));
#4328=CARTESIAN_POINT('Origin',(0.,0.,-2.));
#4329=CARTESIAN_POINT('Origin',(0.,0.,-2.));
#4330=CARTESIAN_POINT('Origin',(0.,0.,0.));
#4331=CARTESIAN_POINT('',(-4.,-4.89858719658941E-16,0.));
#4332=CARTESIAN_POINT('Origin',(0.,0.,20.));
#4333=CARTESIAN_POINT('',(0.,0.,0.));
#4334=CARTESIAN_POINT('Origin',(0.,0.,20.5));
#4335=CARTESIAN_POINT('',(-3.,-3.67394039744206E-16,20.));
#4336=CARTESIAN_POINT('Origin',(0.,0.,20.));
#4337=CARTESIAN_POINT('',(-3.,-3.67394039744206E-16,21.));
#4338=CARTESIAN_POINT('',(-3.,-3.67394039744206E-16,20.5));
#4339=CARTESIAN_POINT('Origin',(0.,0.,21.));
#4340=CARTESIAN_POINT('Origin',(7.,0.,20.));
#4341=CARTESIAN_POINT('',(-4.,4.89858719658941E-16,20.));
#4342=CARTESIAN_POINT('Origin',(0.,0.,20.));
#4343=CARTESIAN_POINT('Origin',(3.,0.,21.));
#4344=CARTESIAN_POINT('',(-4.,-4.89858719658941E-16,21.));
#4345=CARTESIAN_POINT('Origin',(0.,0.,21.));
#4346=CARTESIAN_POINT('Origin',(0.,0.,0.));
#4347=CARTESIAN_POINT('',(-4.,-4.89858719658941E-16,22.));
#4348=CARTESIAN_POINT('Origin',(0.,0.,22.));
#4349=CARTESIAN_POINT('',(-4.,-4.89858719658941E-16,0.));
#4350=CARTESIAN_POINT('Origin',(0.,0.,0.));
#4351=CARTESIAN_POINT('',(-6.,-7.34788079488412E-16,0.));
#4352=CARTESIAN_POINT('Origin',(0.,0.,0.));
#4353=CARTESIAN_POINT('',(-4.,-4.89858719658941E-16,0.));
#4354=CARTESIAN_POINT('Origin',(0.,0.,0.));
#4355=CARTESIAN_POINT('Origin',(0.,0.,-2.));
#4356=CARTESIAN_POINT('',(-6.,-7.34788079488412E-16,-2.));
#4357=CARTESIAN_POINT('',(-6.,-7.34788079488412E-16,-2.));
#4358=CARTESIAN_POINT('Origin',(0.,0.,-2.));
#4359=CARTESIAN_POINT('Origin',(0.,0.,-2.));
#4360=CARTESIAN_POINT('Origin',(0.,0.,0.));
#4361=CARTESIAN_POINT('',(-4.,-4.89858719658941E-16,0.));
#4362=CARTESIAN_POINT('Origin',(0.,0.,22.));
#4363=CARTESIAN_POINT('',(0.,0.,0.));
#4364=CARTESIAN_POINT('Origin',(-1.,0.,1.));
#4365=CARTESIAN_POINT('',(-1.,3.87298334620742,0.));
#4366=CARTESIAN_POINT('',(-1.,3.87298334620742,1.));
#4367=CARTESIAN_POINT('',(-1.,3.87298334620742,0.));
#4368=CARTESIAN_POINT('',(-1.,7.93725393319377,0.));
#4369=CARTESIAN_POINT('',(-1.,0.,0.));
#4370=CARTESIAN_POINT('',(-1.,7.93725393319377,1.));
#4371=CARTESIAN_POINT('',(-1.,7.93725393319377,0.));
#4372=CARTESIAN_POINT('',(-1.,0.,1.));
#4373=CARTESIAN_POINT('Origin',(1.,16.,1.));
#4374=CARTESIAN_POINT('',(1.,3.87298334620742,1.));
#4375=CARTESIAN_POINT('',(1.,3.87298334620742,0.));
#4376=CARTESIAN_POINT('',(1.,3.87298334620742,0.));
#4377=CARTESIAN_POINT('',(1.,7.93725393319377,1.));
#4378=CARTESIAN_POINT('',(1.,8.,1.));
#4379=CARTESIAN_POINT('',(1.,7.93725393319377,0.));
#4380=CARTESIAN_POINT('',(1.,7.93725393319377,0.));
#4381=CARTESIAN_POINT('',(1.,8.,0.));
#4382=CARTESIAN_POINT('Origin',(0.,0.,0.));
#4383=CARTESIAN_POINT('Origin',(0.,0.,0.));
#4384=CARTESIAN_POINT('Origin',(0.,0.,0.));
#4385=CARTESIAN_POINT('Origin',(0.,0.,0.));
#4386=CARTESIAN_POINT('Origin',(0.,0.,1.));
#4387=CARTESIAN_POINT('Origin',(0.,0.,0.));
#4388=CARTESIAN_POINT('Origin',(0.,0.,1.));
#4389=CARTESIAN_POINT('Origin',(0.,0.,1.));
#4390=CARTESIAN_POINT('',(0.,0.,0.));
#4391=CARTESIAN_POINT('Origin',(50.,12.,3.));
#4392=CARTESIAN_POINT('',(45.,12.,6.));
#4393=CARTESIAN_POINT('Origin',(50.,12.,6.));
#4394=CARTESIAN_POINT('',(45.,12.,0.));
#4395=CARTESIAN_POINT('',(45.,12.,3.));
#4396=CARTESIAN_POINT('Origin',(50.,12.,0.));
#4397=CARTESIAN_POINT('Origin',(40.,4.,0.));
#4398=CARTESIAN_POINT('',(40.,4.,0.));
#4399=CARTESIAN_POINT('',(40.,0.,0.));
#4400=CARTESIAN_POINT('',(40.,4.,0.));
#4401=CARTESIAN_POINT('',(40.,0.,6.));
#4402=CARTESIAN_POINT('',(40.,0.,0.));
#4403=CARTESIAN_POINT('',(40.,4.,6.));
#4404=CARTESIAN_POINT('',(40.,4.,6.));
#4405=CARTESIAN_POINT('',(40.,4.,0.));
#4406=CARTESIAN_POINT('Origin',(44.,10.,0.));
#4407=CARTESIAN_POINT('',(44.,10.,0.));
#4408=CARTESIAN_POINT('',(44.,10.,0.));
#4409=CARTESIAN_POINT('',(44.,10.,6.));
#4410=CARTESIAN_POINT('',(44.,10.,6.));
#4411=CARTESIAN_POINT('',(44.,10.,0.));
#4412=CARTESIAN_POINT('Origin',(44.,16.,0.));
#4413=CARTESIAN_POINT('',(44.,16.,0.));
#4414=CARTESIAN_POINT('',(44.,16.,0.));
#4415=CARTESIAN_POINT('',(44.,16.,6.));
#4416=CARTESIAN_POINT('',(44.,16.,6.));
#4417=CARTESIAN_POINT('',(44.,16.,0.));
#4418=CARTESIAN_POINT('Origin',(48.,20.,0.));
#4419=CARTESIAN_POINT('',(48.,20.,0.));
#4420=CARTESIAN_POINT('',(48.,20.,0.));
#4421=CARTESIAN_POINT('',(48.,20.,6.));
#4422=CARTESIAN_POINT('',(48.,20.,6.));
#4423=CARTESIAN_POINT('',(48.,20.,0.));
#4424=CARTESIAN_POINT('Origin',(62.,20.,0.));
#4425=CARTESIAN_POINT('',(62.,20.,0.));
#4426=CARTESIAN_POINT('',(62.,20.,0.));
#4427=CARTESIAN_POINT('',(62.,20.,6.));
#4428=CARTESIAN_POINT('',(62.,20.,6.));
#4429=CARTESIAN_POINT('',(62.,20.,0.));
#4430=CARTESIAN_POINT('Origin',(62.,24.,0.));
#4431=CARTESIAN_POINT('',(62.,24.,0.));
#4432=CARTESIAN_POINT('',(62.,24.,0.));
#4433=CARTESIAN_POINT('',(62.,24.,6.));
#4434=CARTESIAN_POINT('',(62.,24.,6.));
#4435=CARTESIAN_POINT('',(62.,24.,0.));
#4436=CARTESIAN_POINT('Origin',(82.,24.,0.));
#4437=CARTESIAN_POINT('',(82.,24.,0.));
#4438=CARTESIAN_POINT('',(82.,24.,0.));
#4439=CARTESIAN_POINT('',(82.,24.,6.));
#4440=CARTESIAN_POINT('',(82.,24.,6.));
#4441=CARTESIAN_POINT('',(82.,24.,0.));
#4442=CARTESIAN_POINT('Origin',(82.,-2.,0.));
#4443=CARTESIAN_POINT('',(82.,-2.,0.));
#4444=CARTESIAN_POINT('',(82.,-2.,0.));
#4445=CARTESIAN_POINT('',(82.,-2.,6.));
#4446=CARTESIAN_POINT('',(82.,-2.,6.));
#4447=CARTESIAN_POINT('',(82.,-2.,0.));
#4448=CARTESIAN_POINT('Origin',(62.,-2.,0.));
#4449=CARTESIAN_POINT('',(62.,-2.,0.));
#4450=CARTESIAN_POINT('',(62.,-2.,0.));
#4451=CARTESIAN_POINT('',(62.,-2.,6.));
#4452=CARTESIAN_POINT('',(62.,-2.,6.));
#4453=CARTESIAN_POINT('',(62.,-2.,0.));
#4454=CARTESIAN_POINT('Origin',(62.,2.,0.));
#4455=CARTESIAN_POINT('',(62.,2.,0.));
#4456=CARTESIAN_POINT('',(62.,2.,0.));
#4457=CARTESIAN_POINT('',(62.,2.,6.));
#4458=CARTESIAN_POINT('',(62.,2.,6.));
#4459=CARTESIAN_POINT('',(62.,2.,0.));
#4460=CARTESIAN_POINT('Origin',(48.,2.,0.));
#4461=CARTESIAN_POINT('',(48.,2.,0.));
#4462=CARTESIAN_POINT('',(48.,2.,0.));
#4463=CARTESIAN_POINT('',(48.,2.,6.));
#4464=CARTESIAN_POINT('',(48.,2.,6.));
#4465=CARTESIAN_POINT('',(48.,2.,0.));
#4466=CARTESIAN_POINT('Origin',(42.,-3.,0.));
#4467=CARTESIAN_POINT('',(42.,-3.,0.));
#4468=CARTESIAN_POINT('',(42.,-3.,0.));
#4469=CARTESIAN_POINT('',(42.,-3.,6.));
#4470=CARTESIAN_POINT('',(42.,-3.,6.));
#4471=CARTESIAN_POINT('',(42.,-3.,0.));
#4472=CARTESIAN_POINT('Origin',(35.,-3.,0.));
#4473=CARTESIAN_POINT('',(35.,-3.,0.));
#4474=CARTESIAN_POINT('',(35.,-3.,0.));
#4475=CARTESIAN_POINT('',(35.,-3.,6.));
#4476=CARTESIAN_POINT('',(35.,-3.,6.));
#4477=CARTESIAN_POINT('',(35.,-3.,0.));
#4478=CARTESIAN_POINT('Origin',(36.,0.,0.));
#4479=CARTESIAN_POINT('',(36.,0.,0.));
#4480=CARTESIAN_POINT('',(36.,0.,0.));
#4481=CARTESIAN_POINT('',(36.,0.,6.));
#4482=CARTESIAN_POINT('',(36.,0.,6.));
#4483=CARTESIAN_POINT('',(36.,0.,0.));
#4484=CARTESIAN_POINT('Origin',(40.,0.,0.));
#4485=CARTESIAN_POINT('',(40.,0.,0.));
#4486=CARTESIAN_POINT('',(40.,0.,6.));
#4487=CARTESIAN_POINT('Origin',(58.5,10.5,6.));
#4488=CARTESIAN_POINT('Origin',(58.5,10.5,0.));
#4489=CARTESIAN_POINT('',(0.,0.,0.));
#4490=CARTESIAN_POINT('Origin',(0.,0.,0.));
#4491=CARTESIAN_POINT('',(-5.,-6.12323399573677E-16,8.));
#4492=CARTESIAN_POINT('Origin',(0.,0.,8.));
#4493=CARTESIAN_POINT('',(-5.,-6.12323399573677E-16,0.));
#4494=CARTESIAN_POINT('',(-5.,-6.12323399573677E-16,0.));
#4495=CARTESIAN_POINT('Origin',(0.,0.,0.));
#4496=CARTESIAN_POINT('Origin',(0.,0.,0.));
#4497=CARTESIAN_POINT('',(-6.,-7.34788079488412E-16,8.));
#4498=CARTESIAN_POINT('Origin',(0.,0.,8.));
#4499=CARTESIAN_POINT('',(-6.,-7.34788079488412E-16,0.));
#4500=CARTESIAN_POINT('',(-6.,-7.34788079488412E-16,0.));
#4501=CARTESIAN_POINT('Origin',(0.,0.,0.));
#4502=CARTESIAN_POINT('Origin',(0.,0.,8.));
#4503=CARTESIAN_POINT('Origin',(0.,0.,0.));
#4504=CARTESIAN_POINT('',(0.,0.,0.));
#4505=CARTESIAN_POINT('Origin',(0.,0.,0.));
#4506=CARTESIAN_POINT('',(-4.,-4.89858719658941E-16,6.));
#4507=CARTESIAN_POINT('Origin',(0.,0.,6.));
#4508=CARTESIAN_POINT('',(-4.,-4.89858719658941E-16,0.));
#4509=CARTESIAN_POINT('',(-4.,-4.89858719658941E-16,0.));
#4510=CARTESIAN_POINT('Origin',(0.,0.,0.));
#4511=CARTESIAN_POINT('Origin',(0.,0.,0.));
#4512=CARTESIAN_POINT('',(-5.,-6.12323399573677E-16,6.));
#4513=CARTESIAN_POINT('Origin',(0.,0.,6.));
#4514=CARTESIAN_POINT('',(-5.,-6.12323399573677E-16,0.));
#4515=CARTESIAN_POINT('',(-5.,-6.12323399573677E-16,0.));
#4516=CARTESIAN_POINT('Origin',(0.,0.,0.));
#4517=CARTESIAN_POINT('Origin',(0.,0.,6.));
#4518=CARTESIAN_POINT('Origin',(0.,0.,0.));
#4519=CARTESIAN_POINT('',(0.,0.,0.));
#4520=CARTESIAN_POINT('Origin',(0.,0.,0.));
#4521=CARTESIAN_POINT('',(-5.,-6.12323399573677E-16,2.));
#4522=CARTESIAN_POINT('Origin',(0.,0.,2.));
#4523=CARTESIAN_POINT('',(-5.,-6.12323399573677E-16,0.));
#4524=CARTESIAN_POINT('',(-5.,-6.12323399573677E-16,0.));
#4525=CARTESIAN_POINT('Origin',(0.,0.,0.));
#4526=CARTESIAN_POINT('Origin',(0.,0.,0.));
#4527=CARTESIAN_POINT('',(-10.,-1.22464679914735E-15,2.));
#4528=CARTESIAN_POINT('Origin',(0.,0.,2.));
#4529=CARTESIAN_POINT('',(-10.,-1.22464679914735E-15,0.));
#4530=CARTESIAN_POINT('',(-10.,-1.22464679914735E-15,0.));
#4531=CARTESIAN_POINT('Origin',(0.,0.,0.));
#4532=CARTESIAN_POINT('Origin',(0.,0.,2.));
#4533=CARTESIAN_POINT('Origin',(0.,0.,0.));
#4534=CARTESIAN_POINT('',(0.,0.,0.));
#4535=CARTESIAN_POINT('Origin',(0.,0.,0.));
#4536=CARTESIAN_POINT('',(-4.,-4.89858719658941E-16,2.));
#4537=CARTESIAN_POINT('Origin',(0.,0.,2.));
#4538=CARTESIAN_POINT('',(-4.,-4.89858719658941E-16,0.));
#4539=CARTESIAN_POINT('',(-4.,-4.89858719658941E-16,0.));
#4540=CARTESIAN_POINT('Origin',(0.,0.,0.));
#4541=CARTESIAN_POINT('Origin',(0.,0.,0.));
#4542=CARTESIAN_POINT('',(-7.,-8.57252759403147E-16,2.));
#4543=CARTESIAN_POINT('Origin',(0.,0.,2.));
#4544=CARTESIAN_POINT('',(-7.,-8.57252759403147E-16,0.));
#4545=CARTESIAN_POINT('',(-7.,-8.57252759403147E-16,0.));
#4546=CARTESIAN_POINT('Origin',(0.,0.,0.));
#4547=CARTESIAN_POINT('Origin',(0.,0.,2.));
#4548=CARTESIAN_POINT('Origin',(0.,0.,0.));
#4549=CARTESIAN_POINT('',(0.,0.,0.));
#4550=CARTESIAN_POINT('Origin',(0.,0.,0.));
#4551=CARTESIAN_POINT('',(-4.,-4.89858719658941E-16,2.));
#4552=CARTESIAN_POINT('Origin',(0.,0.,2.));
#4553=CARTESIAN_POINT('',(-4.,-4.89858719658941E-16,0.));
#4554=CARTESIAN_POINT('',(-4.,-4.89858719658941E-16,0.));
#4555=CARTESIAN_POINT('Origin',(0.,0.,0.));
#4556=CARTESIAN_POINT('Origin',(0.,0.,0.));
#4557=CARTESIAN_POINT('',(-8.,-9.79717439317883E-16,2.));
#4558=CARTESIAN_POINT('Origin',(0.,0.,2.));
#4559=CARTESIAN_POINT('',(-8.,-9.79717439317883E-16,0.));
#4560=CARTESIAN_POINT('',(-8.,-9.79717439317883E-16,0.));
#4561=CARTESIAN_POINT('Origin',(0.,0.,0.));
#4562=CARTESIAN_POINT('Origin',(0.,0.,2.));
#4563=CARTESIAN_POINT('Origin',(0.,0.,0.));
#4564=CARTESIAN_POINT('',(0.,0.,0.));
#4565=CARTESIAN_POINT('Origin',(-1.,0.,1.));
#4566=CARTESIAN_POINT('',(-1.,2.82842712474619,0.));
#4567=CARTESIAN_POINT('',(-1.,2.82842712474619,1.));
#4568=CARTESIAN_POINT('',(-1.,2.82842712474619,0.));
#4569=CARTESIAN_POINT('',(-1.,5.91607978309962,0.));
#4570=CARTESIAN_POINT('',(-1.,0.,0.));
#4571=CARTESIAN_POINT('',(-1.,5.91607978309962,1.));
#4572=CARTESIAN_POINT('',(-1.,5.91607978309962,0.));
#4573=CARTESIAN_POINT('',(-1.,0.,1.));
#4574=CARTESIAN_POINT('Origin',(1.,12.,1.));
#4575=CARTESIAN_POINT('',(1.,2.82842712474619,1.));
#4576=CARTESIAN_POINT('',(1.,2.82842712474619,0.));
#4577=CARTESIAN_POINT('',(1.,2.82842712474619,0.));
#4578=CARTESIAN_POINT('',(1.,5.91607978309962,1.));
#4579=CARTESIAN_POINT('',(1.,6.,1.));
#4580=CARTESIAN_POINT('',(1.,5.91607978309962,0.));
#4581=CARTESIAN_POINT('',(1.,5.91607978309962,0.));
#4582=CARTESIAN_POINT('',(1.,6.,0.));
#4583=CARTESIAN_POINT('Origin',(0.,0.,0.));
#4584=CARTESIAN_POINT('Origin',(0.,0.,0.));
#4585=CARTESIAN_POINT('Origin',(0.,0.,0.));
#4586=CARTESIAN_POINT('Origin',(0.,0.,0.));
#4587=CARTESIAN_POINT('Origin',(0.,0.,1.));
#4588=CARTESIAN_POINT('Origin',(0.,0.,0.));
#4589=CARTESIAN_POINT('Origin',(0.,0.,1.));
#4590=CARTESIAN_POINT('Origin',(0.,0.,1.));
#4591=CARTESIAN_POINT('',(0.,0.,100.));
#4592=CARTESIAN_POINT('',(-2.5951463200613E-14,-10.,100.));
#4593=CARTESIAN_POINT('',(0.,-20.,100.));
#4594=CARTESIAN_POINT('',(0.,-12.,100.));
#4595=CARTESIAN_POINT('',(0.,0.,100.));
#4596=CARTESIAN_POINT('',(50.,-12.,112.));
#4597=CARTESIAN_POINT('',(26.8635279142892,0.,56.1553781177417));
#4598=CARTESIAN_POINT('',(-2.5951463200613E-14,-10.,100.));
#4599=CARTESIAN_POINT('',(50.,-12.,112.));
#4600=CARTESIAN_POINT('',(0.,-18.,100.));
#4601=CARTESIAN_POINT('',(50.,-18.,112.));
#4602=CARTESIAN_POINT('',(50.,-28.,112.));
#4603=CARTESIAN_POINT('',(0.,-30.,100.));
#4604=CARTESIAN_POINT('',(50.,-30.,112.));
#4605=CARTESIAN_POINT('',(-0.234379292698632,-12.,99.8555317216079));
#4606=CARTESIAN_POINT('',(0.,-20.,100.));
#4607=CARTESIAN_POINT('',(26.8635279142891,-12.,56.1553781177419));
#4608=CARTESIAN_POINT('',(0.,-28.,100.));
#4609=CARTESIAN_POINT('',(26.8635279142892,-10.,56.1553781177417));
#4610=CARTESIAN_POINT('',(26.8635279142892,-18.,56.1553781177417));
#4611=CARTESIAN_POINT('',(26.8635279142892,-20.,56.1553781177417));
#4612=UNCERTAINTY_MEASURE_WITH_UNIT(LENGTH_MEASURE(0.01),#4644,
'DISTANCE_ACCURACY_VALUE',
'Maximum model space distance between geometric entities at asserted c
onnectivities');
#4613=UNCERTAINTY_MEASURE_WITH_UNIT(LENGTH_MEASURE(0.01),#4644,
'DISTANCE_ACCURACY_VALUE',
'Maximum model space distance between geometric entities at asserted c
onnectivities');
#4614=UNCERTAINTY_MEASURE_WITH_UNIT(LENGTH_MEASURE(0.01),#4644,
'DISTANCE_ACCURACY_VALUE',
'Maximum model space distance between geometric entities at asserted c
onnectivities');
#4615=UNCERTAINTY_MEASURE_WITH_UNIT(LENGTH_MEASURE(0.01),#4644,
'DISTANCE_ACCURACY_VALUE',
'Maximum model space distance between geometric entities at asserted c
onnectivities');
#4616=UNCERTAINTY_MEASURE_WITH_UNIT(LENGTH_MEASURE(0.01),#4644,
'DISTANCE_ACCURACY_VALUE',
'Maximum model space distance between geometric entities at asserted c
onnectivities');
#4617=UNCERTAINTY_MEASURE_WITH_UNIT(LENGTH_MEASURE(0.01),#4644,
'DISTANCE_ACCURACY_VALUE',
'Maximum model space distance between geometric entities at asserted c
onnectivities');
#4618=UNCERTAINTY_MEASURE_WITH_UNIT(LENGTH_MEASURE(0.01),#4644,
'DISTANCE_ACCURACY_VALUE',
'Maximum model space distance between geometric entities at asserted c
onnectivities');
#4619=UNCERTAINTY_MEASURE_WITH_UNIT(LENGTH_MEASURE(0.01),#4644,
'DISTANCE_ACCURACY_VALUE',
'Maximum model space distance between geometric entities at asserted c
onnectivities');
#4620=UNCERTAINTY_MEASURE_WITH_UNIT(LENGTH_MEASURE(0.01),#4644,
'DISTANCE_ACCURACY_VALUE',
'Maximum model space distance between geometric entities at asserted c
onnectivities');
#4621=UNCERTAINTY_MEASURE_WITH_UNIT(LENGTH_MEASURE(0.01),#4644,
'DISTANCE_ACCURACY_VALUE',
'Maximum model space distance between geometric entities at asserted c
onnectivities');
#4622=UNCERTAINTY_MEASURE_WITH_UNIT(LENGTH_MEASURE(0.01),#4644,
'DISTANCE_ACCURACY_VALUE',
'Maximum model space distance between geometric entities at asserted c
onnectivities');
#4623=UNCERTAINTY_MEASURE_WITH_UNIT(LENGTH_MEASURE(0.01),#4644,
'DISTANCE_ACCURACY_VALUE',
'Maximum model space distance between geometric entities at asserted c
onnectivities');
#4624=UNCERTAINTY_MEASURE_WITH_UNIT(LENGTH_MEASURE(0.01),#4644,
'DISTANCE_ACCURACY_VALUE',
'Maximum model space distance between geometric entities at asserted c
onnectivities');
#4625=UNCERTAINTY_MEASURE_WITH_UNIT(LENGTH_MEASURE(0.01),#4644,
'DISTANCE_ACCURACY_VALUE',
'Maximum model space distance between geometric entities at asserted c
onnectivities');
#4626=UNCERTAINTY_MEASURE_WITH_UNIT(LENGTH_MEASURE(0.01),#4644,
'DISTANCE_ACCURACY_VALUE',
'Maximum model space distance between geometric entities at asserted c
onnectivities');
#4627=UNCERTAINTY_MEASURE_WITH_UNIT(LENGTH_MEASURE(0.01),#4644,
'DISTANCE_ACCURACY_VALUE',
'Maximum model space distance between geometric entities at asserted c
onnectivities');
#4628=(
GEOMETRIC_REPRESENTATION_CONTEXT(3)
GLOBAL_UNCERTAINTY_ASSIGNED_CONTEXT((#4612))
GLOBAL_UNIT_ASSIGNED_CONTEXT((#4644,#4646,#4647))
REPRESENTATION_CONTEXT('','3D')
);
#4629=(
GEOMETRIC_REPRESENTATION_CONTEXT(3)
GLOBAL_UNCERTAINTY_ASSIGNED_CONTEXT((#4613))
GLOBAL_UNIT_ASSIGNED_CONTEXT((#4644,#4646,#4647))
REPRESENTATION_CONTEXT('','3D')
);
#4630=(
GEOMETRIC_REPRESENTATION_CONTEXT(3)
GLOBAL_UNCERTAINTY_ASSIGNED_CONTEXT((#4614))
GLOBAL_UNIT_ASSIGNED_CONTEXT((#4644,#4646,#4647))
REPRESENTATION_CONTEXT('','3D')
);
#4631=(
GEOMETRIC_REPRESENTATION_CONTEXT(3)
GLOBAL_UNCERTAINTY_ASSIGNED_CONTEXT((#4615))
GLOBAL_UNIT_ASSIGNED_CONTEXT((#4644,#4646,#4647))
REPRESENTATION_CONTEXT('','3D')
);
#4632=(
GEOMETRIC_REPRESENTATION_CONTEXT(3)
GLOBAL_UNCERTAINTY_ASSIGNED_CONTEXT((#4616))
GLOBAL_UNIT_ASSIGNED_CONTEXT((#4644,#4646,#4647))
REPRESENTATION_CONTEXT('','3D')
);
#4633=(
GEOMETRIC_REPRESENTATION_CONTEXT(3)
GLOBAL_UNCERTAINTY_ASSIGNED_CONTEXT((#4617))
GLOBAL_UNIT_ASSIGNED_CONTEXT((#4644,#4646,#4647))
REPRESENTATION_CONTEXT('','3D')
);
#4634=(
GEOMETRIC_REPRESENTATION_CONTEXT(3)
GLOBAL_UNCERTAINTY_ASSIGNED_CONTEXT((#4618))
GLOBAL_UNIT_ASSIGNED_CONTEXT((#4644,#4646,#4647))
REPRESENTATION_CONTEXT('','3D')
);
#4635=(
GEOMETRIC_REPRESENTATION_CONTEXT(3)
GLOBAL_UNCERTAINTY_ASSIGNED_CONTEXT((#4619))
GLOBAL_UNIT_ASSIGNED_CONTEXT((#4644,#4646,#4647))
REPRESENTATION_CONTEXT('','3D')
);
#4636=(
GEOMETRIC_REPRESENTATION_CONTEXT(3)
GLOBAL_UNCERTAINTY_ASSIGNED_CONTEXT((#4620))
GLOBAL_UNIT_ASSIGNED_CONTEXT((#4644,#4646,#4647))
REPRESENTATION_CONTEXT('','3D')
);
#4637=(
GEOMETRIC_REPRESENTATION_CONTEXT(3)
GLOBAL_UNCERTAINTY_ASSIGNED_CONTEXT((#4621))
GLOBAL_UNIT_ASSIGNED_CONTEXT((#4644,#4646,#4647))
REPRESENTATION_CONTEXT('','3D')
);
#4638=(
GEOMETRIC_REPRESENTATION_CONTEXT(3)
GLOBAL_UNCERTAINTY_ASSIGNED_CONTEXT((#4622))
GLOBAL_UNIT_ASSIGNED_CONTEXT((#4644,#4646,#4647))
REPRESENTATION_CONTEXT('','3D')
);
#4639=(
GEOMETRIC_REPRESENTATION_CONTEXT(3)
GLOBAL_UNCERTAINTY_ASSIGNED_CONTEXT((#4623))
GLOBAL_UNIT_ASSIGNED_CONTEXT((#4644,#4646,#4647))
REPRESENTATION_CONTEXT('','3D')
);
#4640=(
GEOMETRIC_REPRESENTATION_CONTEXT(3)
GLOBAL_UNCERTAINTY_ASSIGNED_CONTEXT((#4624))
GLOBAL_UNIT_ASSIGNED_CONTEXT((#4644,#4646,#4647))
REPRESENTATION_CONTEXT('','3D')
);
#4641=(
GEOMETRIC_REPRESENTATION_CONTEXT(3)
GLOBAL_UNCERTAINTY_ASSIGNED_CONTEXT((#4625))
GLOBAL_UNIT_ASSIGNED_CONTEXT((#4644,#4646,#4647))
REPRESENTATION_CONTEXT('','3D')
);
#4642=(
GEOMETRIC_REPRESENTATION_CONTEXT(3)
GLOBAL_UNCERTAINTY_ASSIGNED_CONTEXT((#4626))
GLOBAL_UNIT_ASSIGNED_CONTEXT((#4644,#4646,#4647))
REPRESENTATION_CONTEXT('','3D')
);
#4643=(
GEOMETRIC_REPRESENTATION_CONTEXT(3)
GLOBAL_UNCERTAINTY_ASSIGNED_CONTEXT((#4627))
GLOBAL_UNIT_ASSIGNED_CONTEXT((#4644,#4646,#4647))
REPRESENTATION_CONTEXT('','3D')
);
#4644=(
LENGTH_UNIT()
NAMED_UNIT(*)
SI_UNIT(.MILLI.,.METRE.)
);
#4645=(
LENGTH_UNIT()
NAMED_UNIT(*)
SI_UNIT($,.METRE.)
);
#4646=(
NAMED_UNIT(*)
PLANE_ANGLE_UNIT()
SI_UNIT($,.RADIAN.)
);
#4647=(
NAMED_UNIT(*)
SI_UNIT($,.STERADIAN.)
SOLID_ANGLE_UNIT()
);
#4648=SHAPE_DEFINITION_REPRESENTATION(#4663,#4699);
#4649=SHAPE_DEFINITION_REPRESENTATION(#4664,#4700);
#4650=SHAPE_DEFINITION_REPRESENTATION(#4665,#4701);
#4651=SHAPE_DEFINITION_REPRESENTATION(#4666,#4702);
#4652=SHAPE_DEFINITION_REPRESENTATION(#4667,#4703);
#4653=SHAPE_DEFINITION_REPRESENTATION(#4668,#4704);
#4654=SHAPE_DEFINITION_REPRESENTATION(#4669,#4705);
#4655=SHAPE_DEFINITION_REPRESENTATION(#4670,#4706);
#4656=SHAPE_DEFINITION_REPRESENTATION(#4671,#4707);
#4657=SHAPE_DEFINITION_REPRESENTATION(#4672,#4708);
#4658=SHAPE_DEFINITION_REPRESENTATION(#4673,#4709);
#4659=SHAPE_DEFINITION_REPRESENTATION(#4674,#4710);
#4660=SHAPE_DEFINITION_REPRESENTATION(#4675,#4711);
#4661=SHAPE_DEFINITION_REPRESENTATION(#4676,#4712);
#4662=SHAPE_DEFINITION_REPRESENTATION(#4677,#4713);
#4663=PRODUCT_DEFINITION_SHAPE('',$,#4715);
#4664=PRODUCT_DEFINITION_SHAPE('',$,#4716);
#4665=PRODUCT_DEFINITION_SHAPE('',$,#4717);
#4666=PRODUCT_DEFINITION_SHAPE('',$,#4718);
#4667=PRODUCT_DEFINITION_SHAPE('',$,#4719);
#4668=PRODUCT_DEFINITION_SHAPE('',$,#4720);
#4669=PRODUCT_DEFINITION_SHAPE('',$,#4721);
#4670=PRODUCT_DEFINITION_SHAPE('',$,#4722);
#4671=PRODUCT_DEFINITION_SHAPE('',$,#4723);
#4672=PRODUCT_DEFINITION_SHAPE('',$,#4724);
#4673=PRODUCT_DEFINITION_SHAPE('',$,#4725);
#4674=PRODUCT_DEFINITION_SHAPE('',$,#4726);
#4675=PRODUCT_DEFINITION_SHAPE('',$,#4727);
#4676=PRODUCT_DEFINITION_SHAPE('',$,#4728);
#4677=PRODUCT_DEFINITION_SHAPE('',$,#4729);
#4678=PRODUCT_DEFINITION_SHAPE($,$,#74);
#4679=PRODUCT_DEFINITION_SHAPE($,$,#75);
#4680=PRODUCT_DEFINITION_SHAPE($,$,#76);
#4681=PRODUCT_DEFINITION_SHAPE($,$,#77);
#4682=PRODUCT_DEFINITION_SHAPE($,$,#78);
#4683=PRODUCT_DEFINITION_SHAPE($,$,#79);
#4684=PRODUCT_DEFINITION_SHAPE($,$,#80);
#4685=PRODUCT_DEFINITION_SHAPE($,$,#81);
#4686=PRODUCT_DEFINITION_SHAPE($,$,#82);
#4687=PRODUCT_DEFINITION_SHAPE($,$,#83);
#4688=PRODUCT_DEFINITION_SHAPE($,$,#84);
#4689=PRODUCT_DEFINITION_SHAPE($,$,#85);
#4690=PRODUCT_DEFINITION_SHAPE($,$,#86);
#4691=PRODUCT_DEFINITION_SHAPE($,$,#87);
#4692=PRODUCT_DEFINITION_SHAPE($,$,#88);
#4693=PRODUCT_DEFINITION_SHAPE($,$,#89);
#4694=PRODUCT_DEFINITION_SHAPE($,$,#90);
#4695=PRODUCT_DEFINITION_SHAPE($,$,#91);
#4696=PRODUCT_DEFINITION_SHAPE($,$,#92);
#4697=PRODUCT_DEFINITION_SHAPE($,$,#93);
#4698=PRODUCT_DEFINITION_SHAPE($,$,#94);
#4699=SHAPE_REPRESENTATION('',(#2828,#3066,#3067,#3068,#3069,#3070,#3071,
#3072,#3073,#3074,#3075,#3076,#3077,#3078,#3079,#3080,#3081,#3082,#3083,
#3084,#3085,#3086),#4628);
#4700=SHAPE_REPRESENTATION('',(#2829),#4629);
#4701=SHAPE_REPRESENTATION('',(#2858),#4630);
#4702=SHAPE_REPRESENTATION('',(#2904),#4631);
#4703=SHAPE_REPRESENTATION('',(#2924),#4632);
#4704=SHAPE_REPRESENTATION('',(#2942),#4633);
#4705=SHAPE_REPRESENTATION('',(#2960),#4634);
#4706=SHAPE_REPRESENTATION('',(#2978),#4635);
#4707=SHAPE_REPRESENTATION('',(#2989),#4636);
#4708=SHAPE_REPRESENTATION('',(#3010),#4637);
#4709=SHAPE_REPRESENTATION('',(#3019),#4638);
#4710=SHAPE_REPRESENTATION('',(#3028),#4639);
#4711=SHAPE_REPRESENTATION('',(#3037),#4640);
#4712=SHAPE_REPRESENTATION('',(#3046),#4641);
#4713=SHAPE_REPRESENTATION('',(#3055),#4642);
#4714=PRODUCT_DEFINITION_CONTEXT('part definition',#4761,'design');
#4715=PRODUCT_DEFINITION('MAS-208','MAS-208',#4730,#4714);
#4716=PRODUCT_DEFINITION('Mounting frame','Mounting frame',#4731,#4714);
#4717=PRODUCT_DEFINITION('Ratchet wheel','Ratchet wheel',#4732,#4714);
#4718=PRODUCT_DEFINITION('Drive lever','Drive lever',#4733,#4714);
#4719=PRODUCT_DEFINITION('Main axle','Main axle',#4734,#4714);
#4720=PRODUCT_DEFINITION('Drive pawl pivot pin','Drive pawl pivot pin',
#4735,#4714);
#4721=PRODUCT_DEFINITION('Holding pawl pivot pin',
'Holding pawl pivot pin',#4736,#4714);
#4722=PRODUCT_DEFINITION('Main retaining ring','Main retaining ring',#4737,
#4714);
#4723=PRODUCT_DEFINITION('Weighted pawl','Weighted pawl',#4738,#4714);
#4724=PRODUCT_DEFINITION('Main bearing sleeve','Main bearing sleeve',#4739,
#4714);
#4725=PRODUCT_DEFINITION('Pawl bearing sleeve','Pawl bearing sleeve',#4740,
#4714);
#4726=PRODUCT_DEFINITION('Main thrust washer','Main thrust washer',#4741,
#4714);
#4727=PRODUCT_DEFINITION('Pawl spacer','Pawl spacer',#4742,#4714);
#4728=PRODUCT_DEFINITION('Pawl thrust washer','Pawl thrust washer',#4743,
#4714);
#4729=PRODUCT_DEFINITION('Pawl retaining ring','Pawl retaining ring',#4744,
#4714);
#4730=PRODUCT_DEFINITION_FORMATION('',$,#4763);
#4731=PRODUCT_DEFINITION_FORMATION('',$,#4764);
#4732=PRODUCT_DEFINITION_FORMATION('',$,#4765);
#4733=PRODUCT_DEFINITION_FORMATION('',$,#4766);
#4734=PRODUCT_DEFINITION_FORMATION('',$,#4767);
#4735=PRODUCT_DEFINITION_FORMATION('',$,#4768);
#4736=PRODUCT_DEFINITION_FORMATION('',$,#4769);
#4737=PRODUCT_DEFINITION_FORMATION('',$,#4770);
#4738=PRODUCT_DEFINITION_FORMATION('',$,#4771);
#4739=PRODUCT_DEFINITION_FORMATION('',$,#4772);
#4740=PRODUCT_DEFINITION_FORMATION('',$,#4773);
#4741=PRODUCT_DEFINITION_FORMATION('',$,#4774);
#4742=PRODUCT_DEFINITION_FORMATION('',$,#4775);
#4743=PRODUCT_DEFINITION_FORMATION('',$,#4776);
#4744=PRODUCT_DEFINITION_FORMATION('',$,#4777);
#4745=PRODUCT_RELATED_PRODUCT_CATEGORY('MAS-208','MAS-208',(#4763));
#4746=PRODUCT_RELATED_PRODUCT_CATEGORY('Mounting frame',
'Mounting frame',(#4764));
#4747=PRODUCT_RELATED_PRODUCT_CATEGORY('Ratchet wheel','Ratchet wheel',
(#4765));
#4748=PRODUCT_RELATED_PRODUCT_CATEGORY('Drive lever','Drive lever',(#4766));
#4749=PRODUCT_RELATED_PRODUCT_CATEGORY('Main axle','Main axle',(#4767));
#4750=PRODUCT_RELATED_PRODUCT_CATEGORY('Drive pawl pivot pin',
'Drive pawl pivot pin',(#4768));
#4751=PRODUCT_RELATED_PRODUCT_CATEGORY('Holding pawl pivot pin',
'Holding pawl pivot pin',(#4769));
#4752=PRODUCT_RELATED_PRODUCT_CATEGORY('Main retaining ring',
'Main retaining ring',(#4770));
#4753=PRODUCT_RELATED_PRODUCT_CATEGORY('Weighted pawl','Weighted pawl',
(#4771));
#4754=PRODUCT_RELATED_PRODUCT_CATEGORY('Main bearing sleeve',
'Main bearing sleeve',(#4772));
#4755=PRODUCT_RELATED_PRODUCT_CATEGORY('Pawl bearing sleeve',
'Pawl bearing sleeve',(#4773));
#4756=PRODUCT_RELATED_PRODUCT_CATEGORY('Main thrust washer',
'Main thrust washer',(#4774));
#4757=PRODUCT_RELATED_PRODUCT_CATEGORY('Pawl spacer','Pawl spacer',(#4775));
#4758=PRODUCT_RELATED_PRODUCT_CATEGORY('Pawl thrust washer',
'Pawl thrust washer',(#4776));
#4759=PRODUCT_RELATED_PRODUCT_CATEGORY('Pawl retaining ring',
'Pawl retaining ring',(#4777));
#4760=APPLICATION_PROTOCOL_DEFINITION('international standard',
'automotive_design',2009,#4761);
#4761=APPLICATION_CONTEXT(
'Core Data for Automotive Mechanical Design Process');
#4762=PRODUCT_CONTEXT('part definition',#4761,'mechanical');
#4763=PRODUCT('MAS-208','MAS-208',
'Independent vertical20-tooth ratchet advance with repeated integral-c
ounterweight gravity pawls, swinging drive lever, bronze sleeves and f
ully retained axle stacks.18degpertooth. Native revolutes; geometric c
ycle checking rather than automatic contact/rolling dynamics. Gravity 
closing checked from actual pawl center of mass. Backplate/foot suppor
ts unit. Fits, torque, holding force, wear and life unassigned.',(#4762));
#4764=PRODUCT('Mounting frame','Mounting frame',$,(#4762));
#4765=PRODUCT('Ratchet wheel','Ratchet wheel','Ratchet wheel',(#4762));
#4766=PRODUCT('Drive lever','Drive lever',$,(#4762));
#4767=PRODUCT('Main axle','Main axle',$,(#4762));
#4768=PRODUCT('Drive pawl pivot pin','Drive pawl pivot pin',$,(#4762));
#4769=PRODUCT('Holding pawl pivot pin','Holding pawl pivot pin',$,(#4762));
#4770=PRODUCT('Main retaining ring','Main retaining ring',$,(#4762));
#4771=PRODUCT('Weighted pawl','Weighted pawl',$,(#4762));
#4772=PRODUCT('Main bearing sleeve','Main bearing sleeve',$,(#4762));
#4773=PRODUCT('Pawl bearing sleeve','Pawl bearing sleeve',$,(#4762));
#4774=PRODUCT('Main thrust washer','Main thrust washer',$,(#4762));
#4775=PRODUCT('Pawl spacer','Pawl spacer',$,(#4762));
#4776=PRODUCT('Pawl thrust washer','Pawl thrust washer',$,(#4762));
#4777=PRODUCT('Pawl retaining ring','Pawl retaining ring',$,(#4762));
#4778=PRESENTATION_STYLE_ASSIGNMENT((#4787));
#4779=PRESENTATION_STYLE_ASSIGNMENT((#4788));
#4780=PRESENTATION_STYLE_ASSIGNMENT((#4789));
#4781=PRESENTATION_STYLE_ASSIGNMENT((#4790));
#4782=PRESENTATION_STYLE_ASSIGNMENT((#4791));
#4783=PRESENTATION_STYLE_ASSIGNMENT((#4792));
#4784=PRESENTATION_STYLE_ASSIGNMENT((#4793));
#4785=PRESENTATION_STYLE_ASSIGNMENT((#4794));
#4786=PRESENTATION_STYLE_ASSIGNMENT((#4795));
#4787=SURFACE_STYLE_USAGE(.BOTH.,#4796);
#4788=SURFACE_STYLE_USAGE(.BOTH.,#4797);
#4789=SURFACE_STYLE_USAGE(.BOTH.,#4798);
#4790=SURFACE_STYLE_USAGE(.BOTH.,#4799);
#4791=SURFACE_STYLE_USAGE(.BOTH.,#4800);
#4792=SURFACE_STYLE_USAGE(.BOTH.,#4801);
#4793=SURFACE_STYLE_USAGE(.BOTH.,#4802);
#4794=SURFACE_STYLE_USAGE(.BOTH.,#4803);
#4795=SURFACE_STYLE_USAGE(.BOTH.,#4804);
#4796=SURFACE_SIDE_STYLE('',(#4805));
#4797=SURFACE_SIDE_STYLE('',(#4806));
#4798=SURFACE_SIDE_STYLE('',(#4807));
#4799=SURFACE_SIDE_STYLE('',(#4808));
#4800=SURFACE_SIDE_STYLE('',(#4809));
#4801=SURFACE_SIDE_STYLE('',(#4810));
#4802=SURFACE_SIDE_STYLE('',(#4811));
#4803=SURFACE_SIDE_STYLE('',(#4812));
#4804=SURFACE_SIDE_STYLE('',(#4813));
#4805=SURFACE_STYLE_FILL_AREA(#4814);
#4806=SURFACE_STYLE_FILL_AREA(#4815);
#4807=SURFACE_STYLE_FILL_AREA(#4816);
#4808=SURFACE_STYLE_FILL_AREA(#4817);
#4809=SURFACE_STYLE_FILL_AREA(#4818);
#4810=SURFACE_STYLE_FILL_AREA(#4819);
#4811=SURFACE_STYLE_FILL_AREA(#4820);
#4812=SURFACE_STYLE_FILL_AREA(#4821);
#4813=SURFACE_STYLE_FILL_AREA(#4822);
#4814=FILL_AREA_STYLE('Steel - Satin',(#4823));
#4815=FILL_AREA_STYLE('Frame gray',(#4824));
#4816=FILL_AREA_STYLE('Dark blue',(#4825));
#4817=FILL_AREA_STYLE('Light blue',(#4826));
#4818=FILL_AREA_STYLE('Axle gray',(#4827));
#4819=FILL_AREA_STYLE('Dark gray',(#4828));
#4820=FILL_AREA_STYLE('Sky blue',(#4829));
#4821=FILL_AREA_STYLE('Bearing light gray',(#4830));
#4822=FILL_AREA_STYLE('Light gray',(#4831));
#4823=FILL_AREA_STYLE_COLOUR('Steel - Satin',#4832);
#4824=FILL_AREA_STYLE_COLOUR('Frame gray',#4833);
#4825=FILL_AREA_STYLE_COLOUR('Dark blue',#4834);
#4826=FILL_AREA_STYLE_COLOUR('Light blue',#4835);
#4827=FILL_AREA_STYLE_COLOUR('Axle gray',#4836);
#4828=FILL_AREA_STYLE_COLOUR('Dark gray',#4837);
#4829=FILL_AREA_STYLE_COLOUR('Sky blue',#4838);
#4830=FILL_AREA_STYLE_COLOUR('Bearing light gray',#4839);
#4831=FILL_AREA_STYLE_COLOUR('Light gray',#4840);
#4832=COLOUR_RGB('Steel - Satin',0.627450980392157,0.627450980392157,0.627450980392157);
#4833=COLOUR_RGB('Frame gray',0.407843137254902,0.447058823529412,0.498039215686275);
#4834=COLOUR_RGB('Dark blue',0.0901960784313725,0.270588235294118,0.513725490196078);
#4835=COLOUR_RGB('Light blue',0.662745098039216,0.831372549019608,0.949019607843137);
#4836=COLOUR_RGB('Axle gray',0.576470588235294,0.615686274509804,0.666666666666667);
#4837=COLOUR_RGB('Dark gray',0.250980392156863,0.282352941176471,0.32156862745098);
#4838=COLOUR_RGB('Sky blue',0.317647058823529,0.686274509803922,0.890196078431372);
#4839=COLOUR_RGB('Bearing light gray',0.725490196078431,0.752941176470588,
0.792156862745098);
#4840=COLOUR_RGB('Light gray',0.725490196078431,0.752941176470588,0.792156862745098);
ENDSEC;
END-ISO-10303-21;
